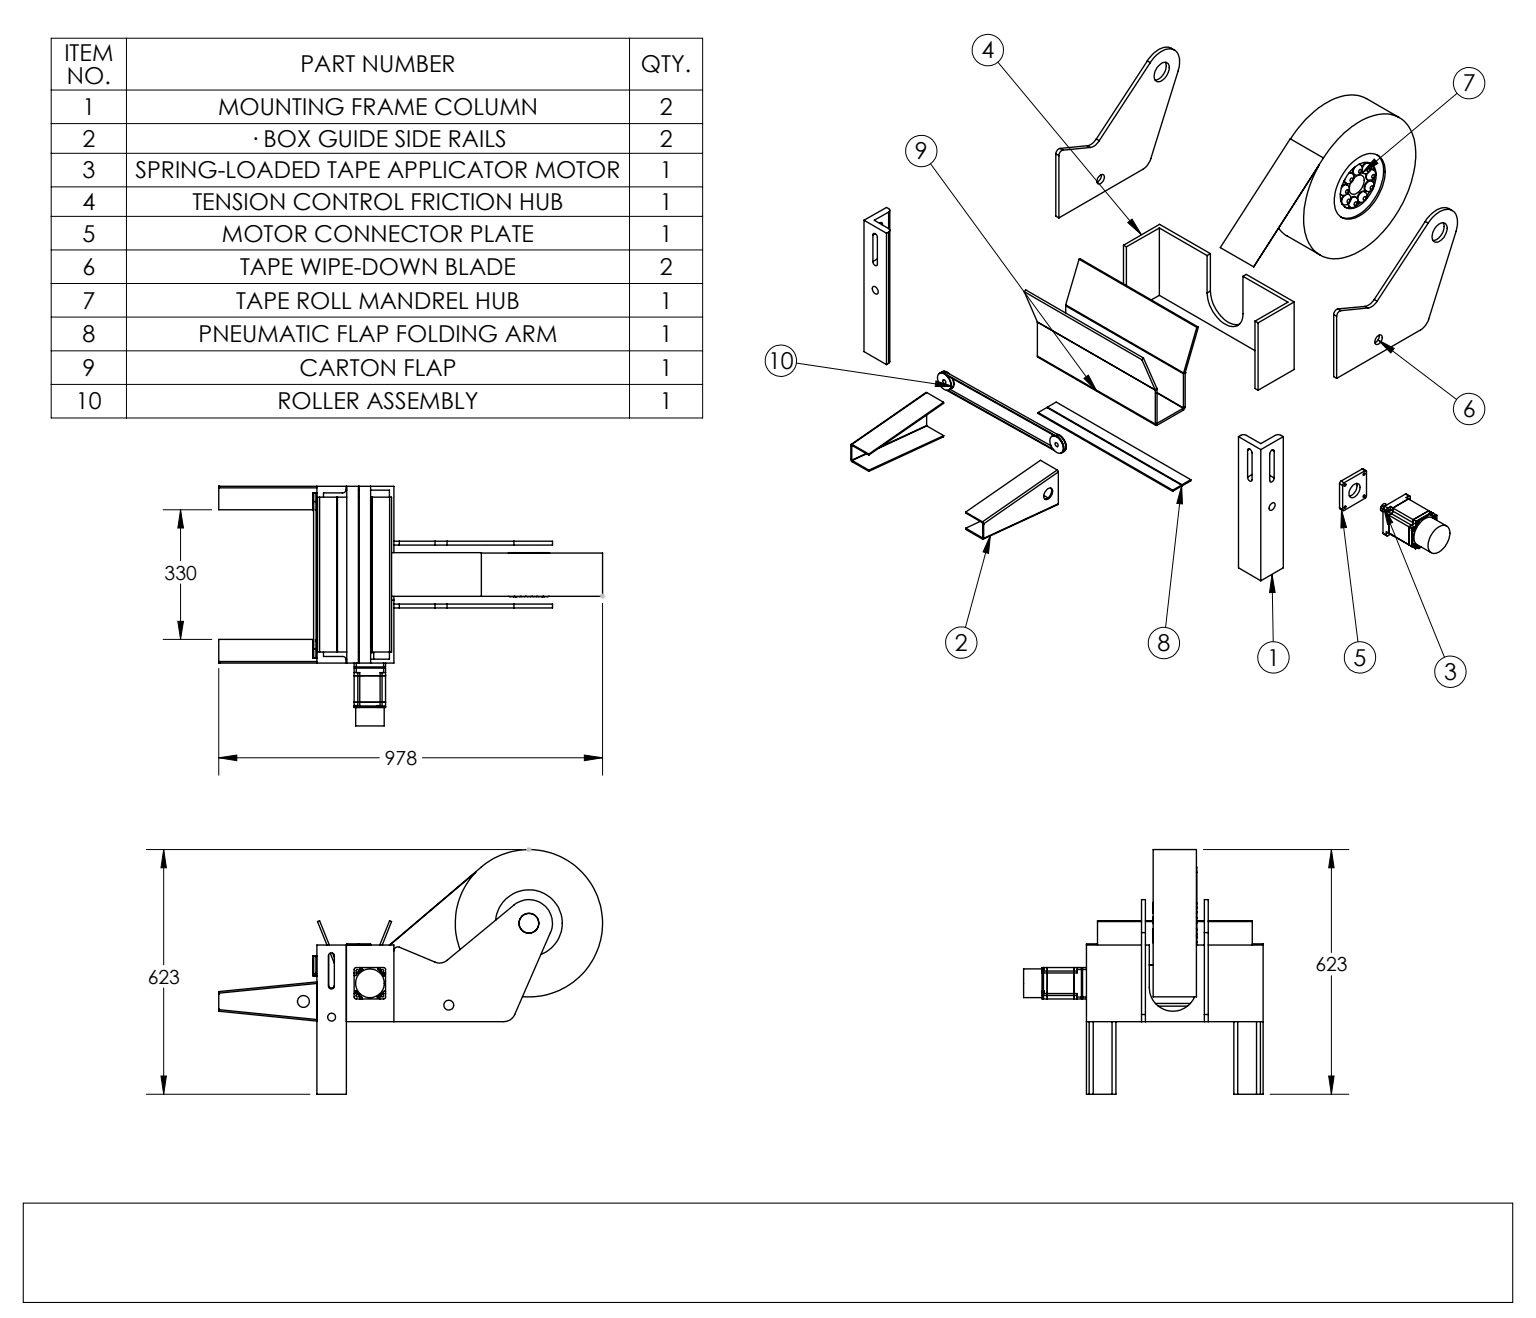
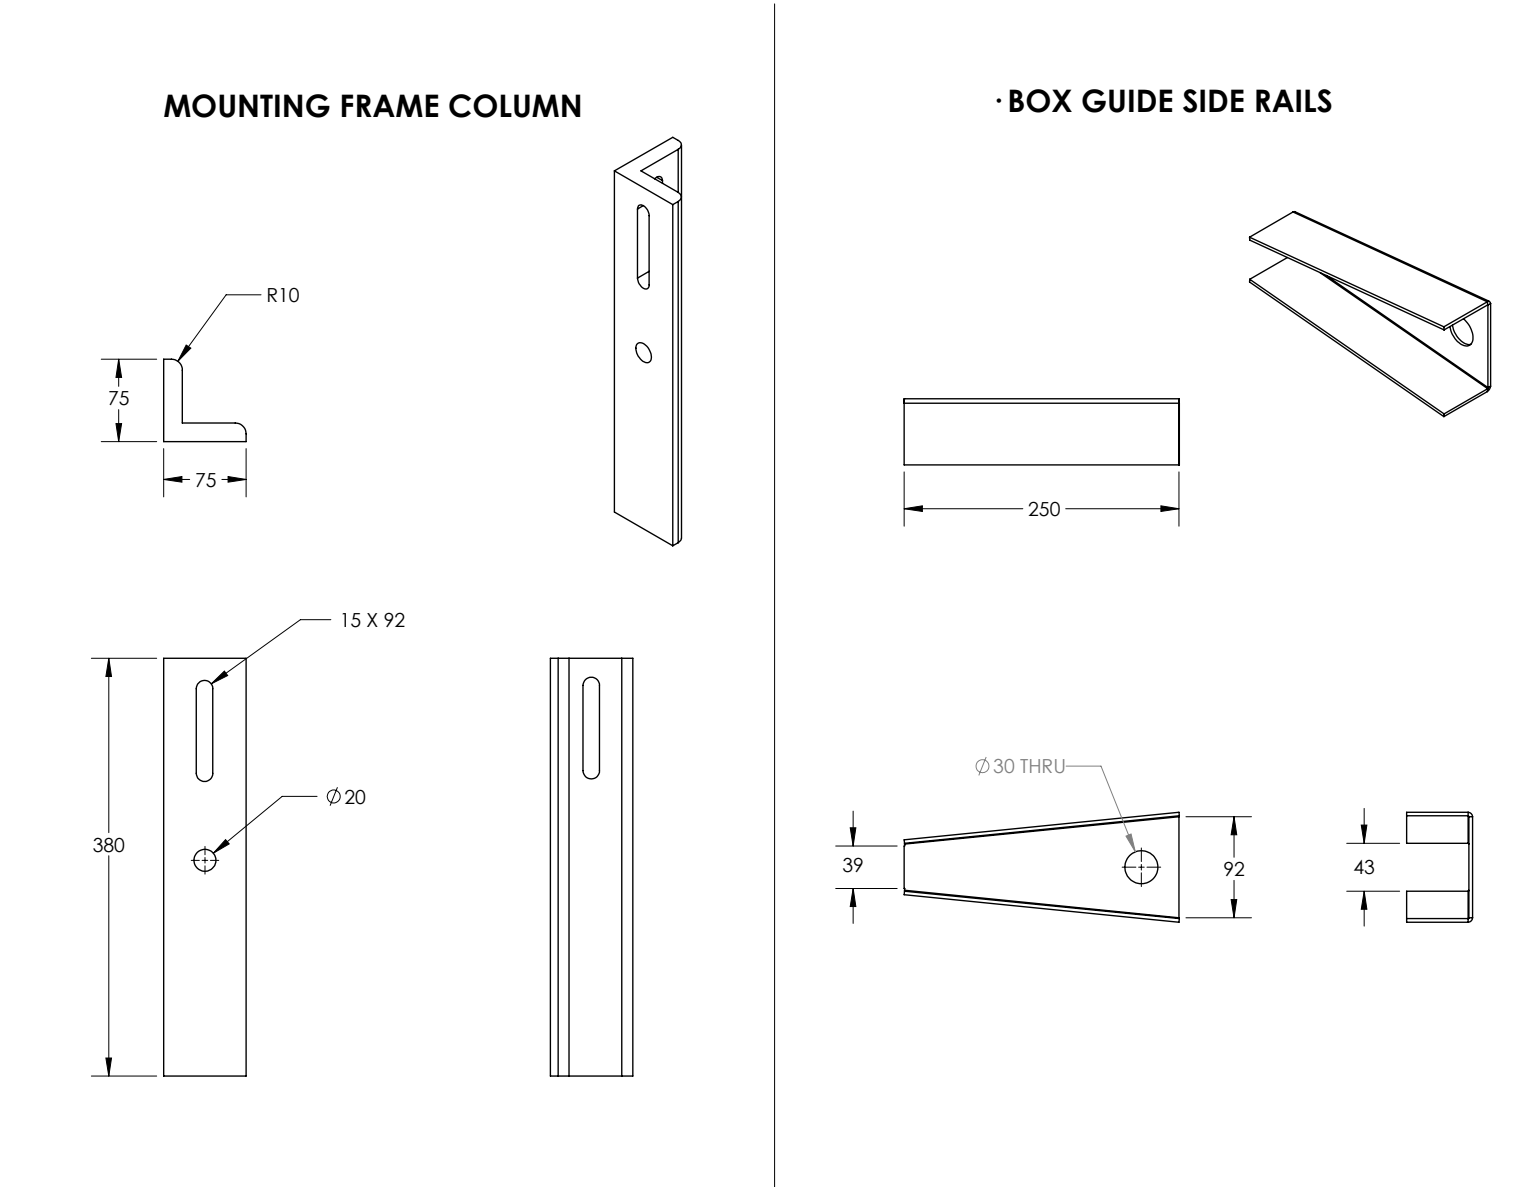
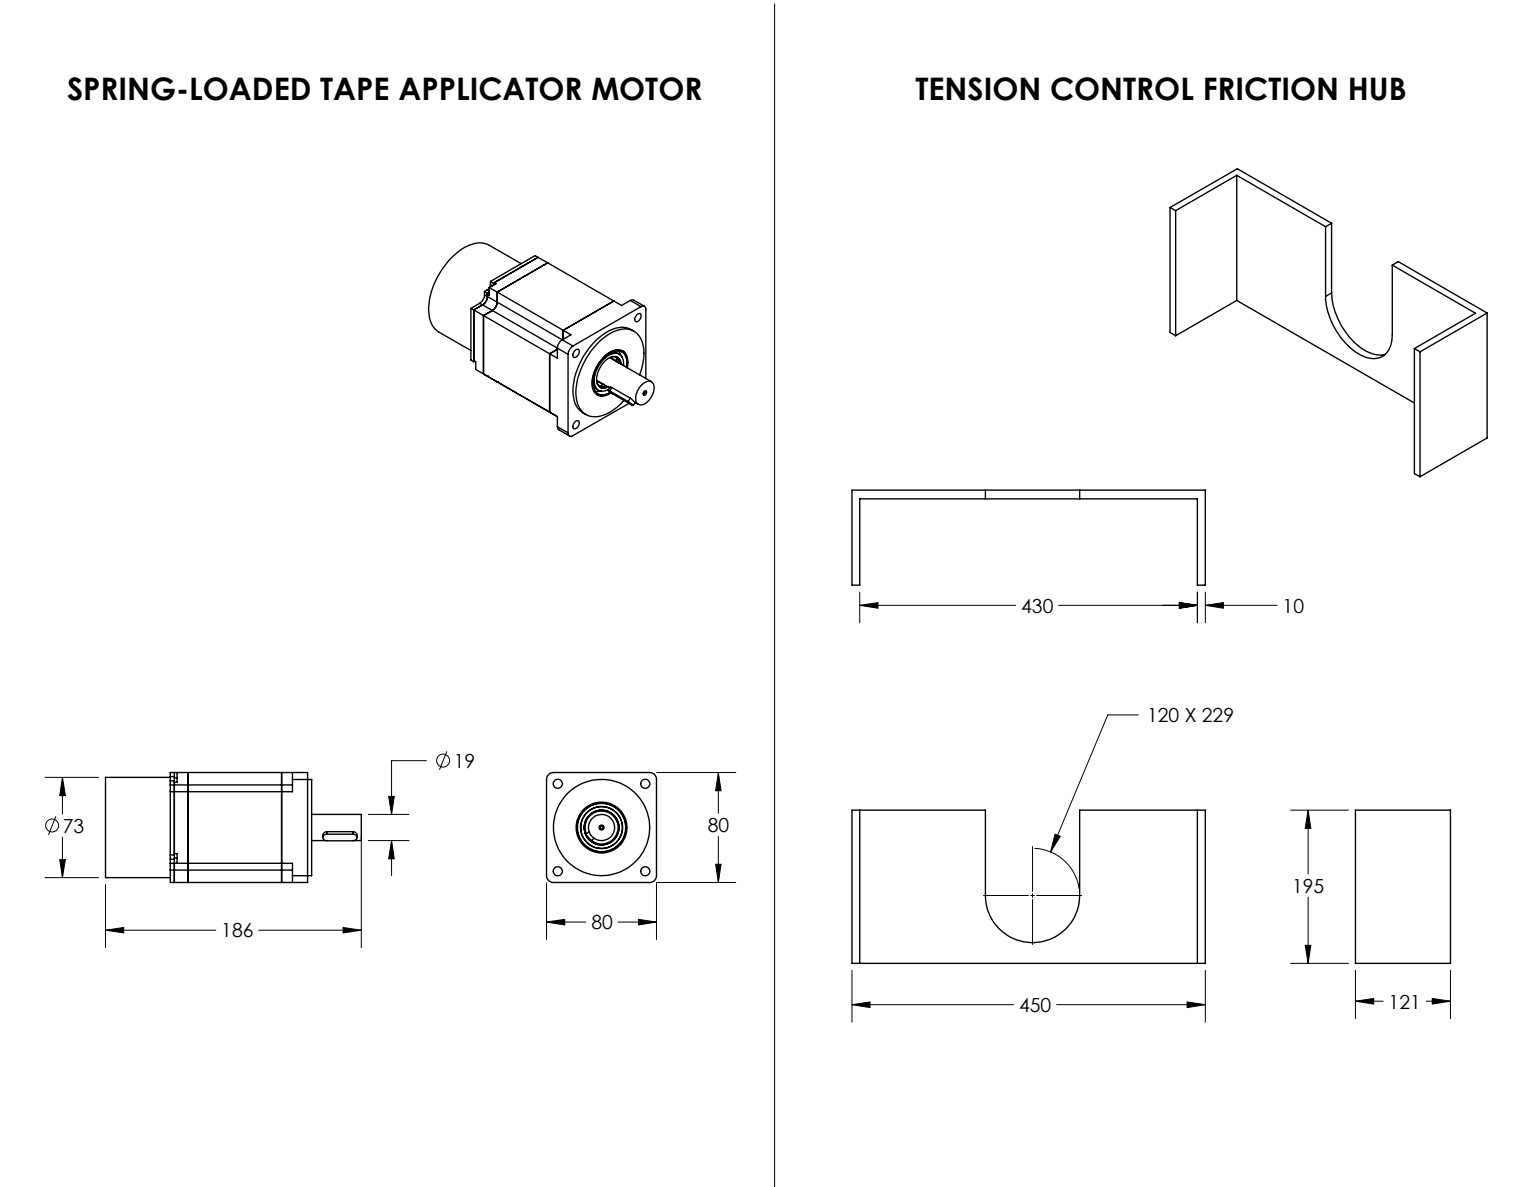
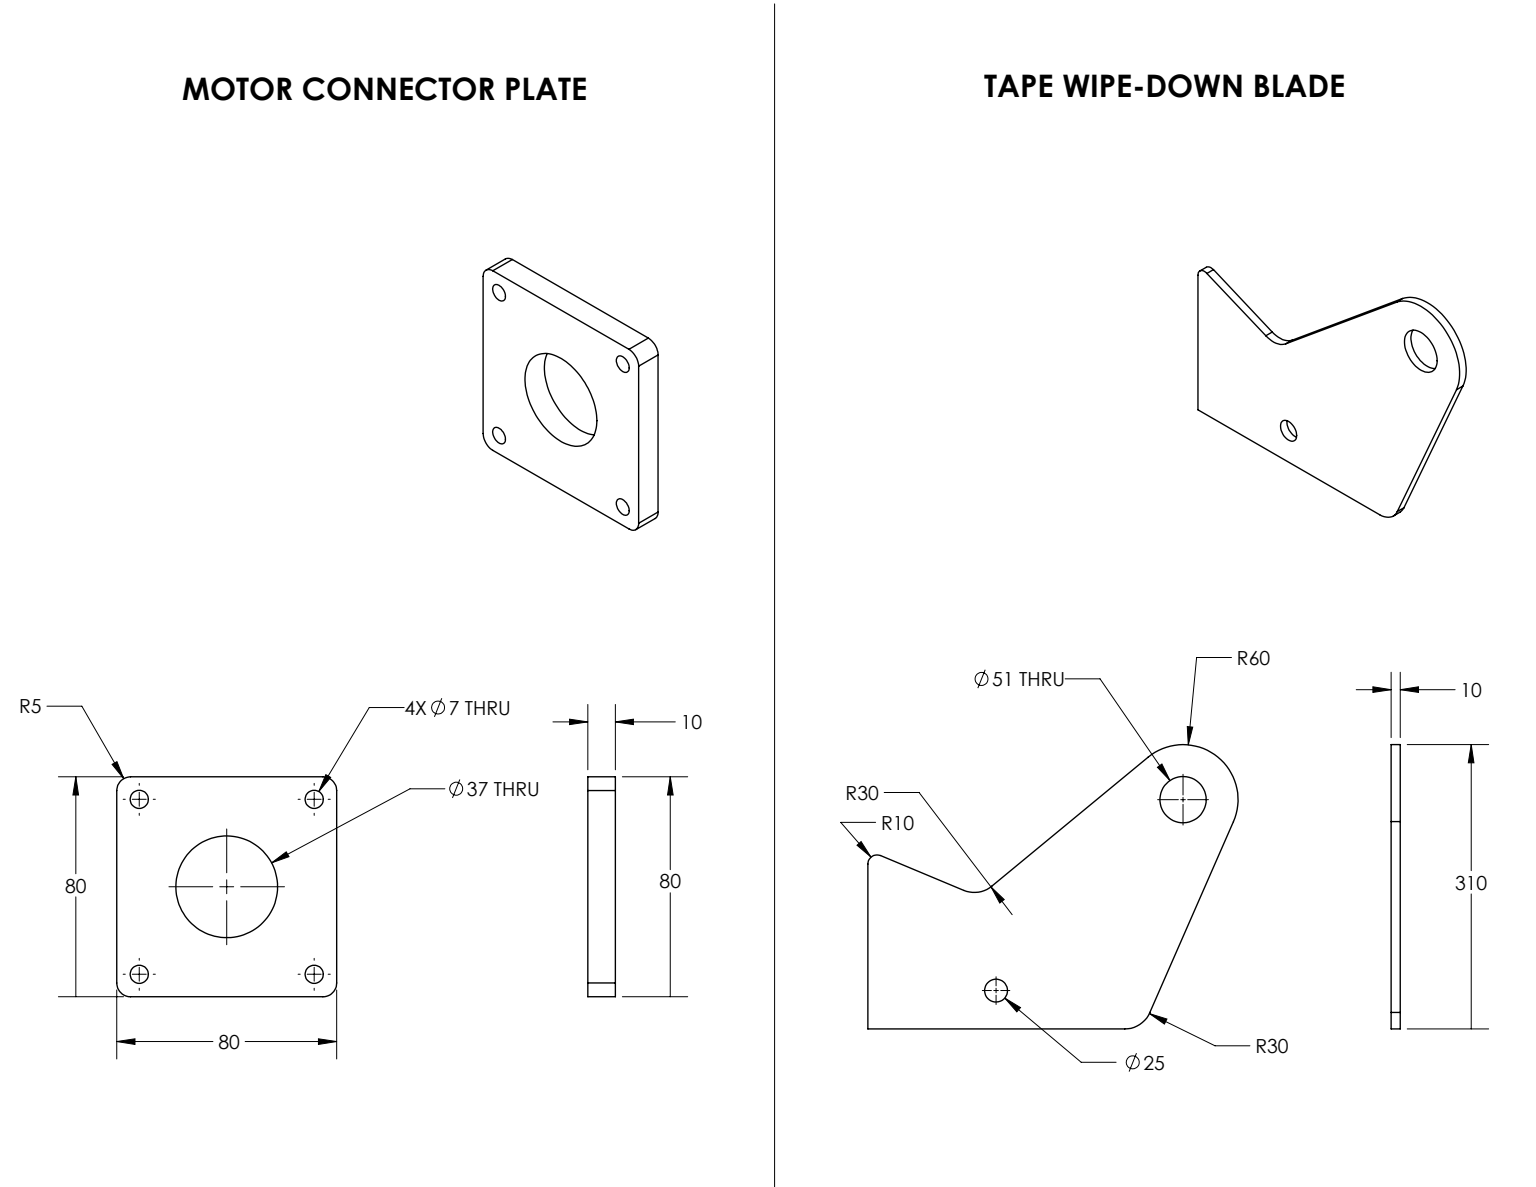
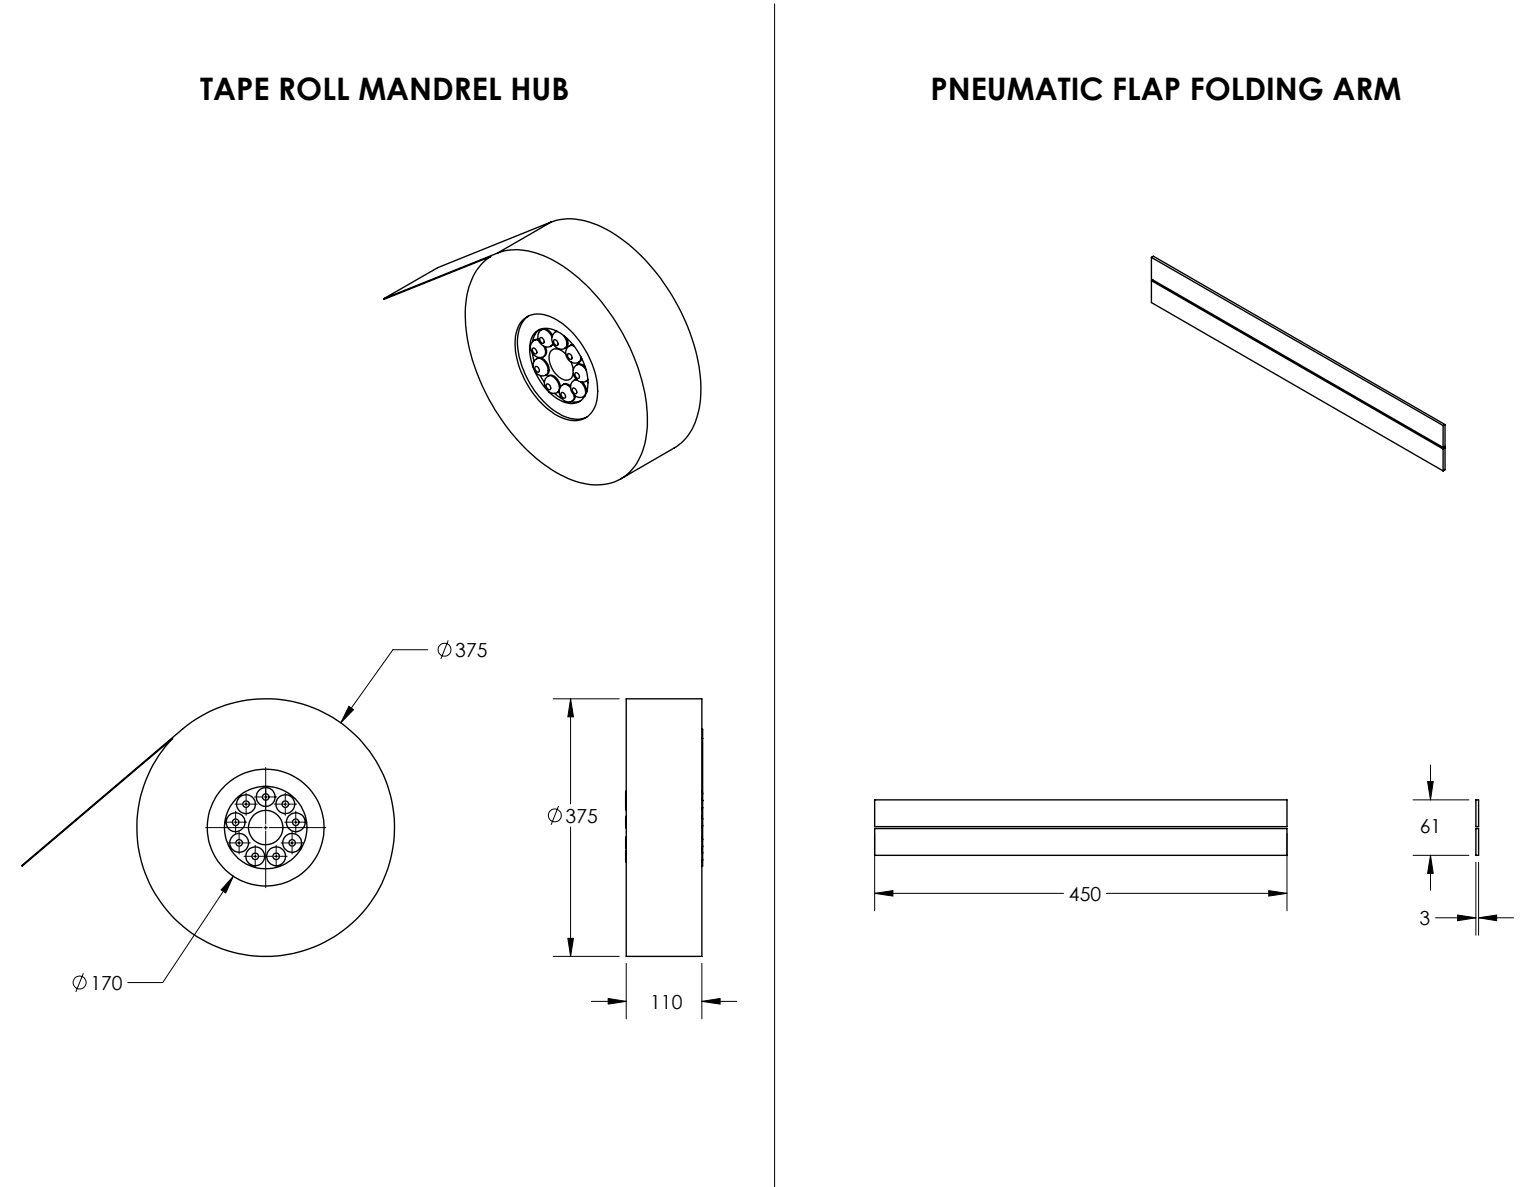
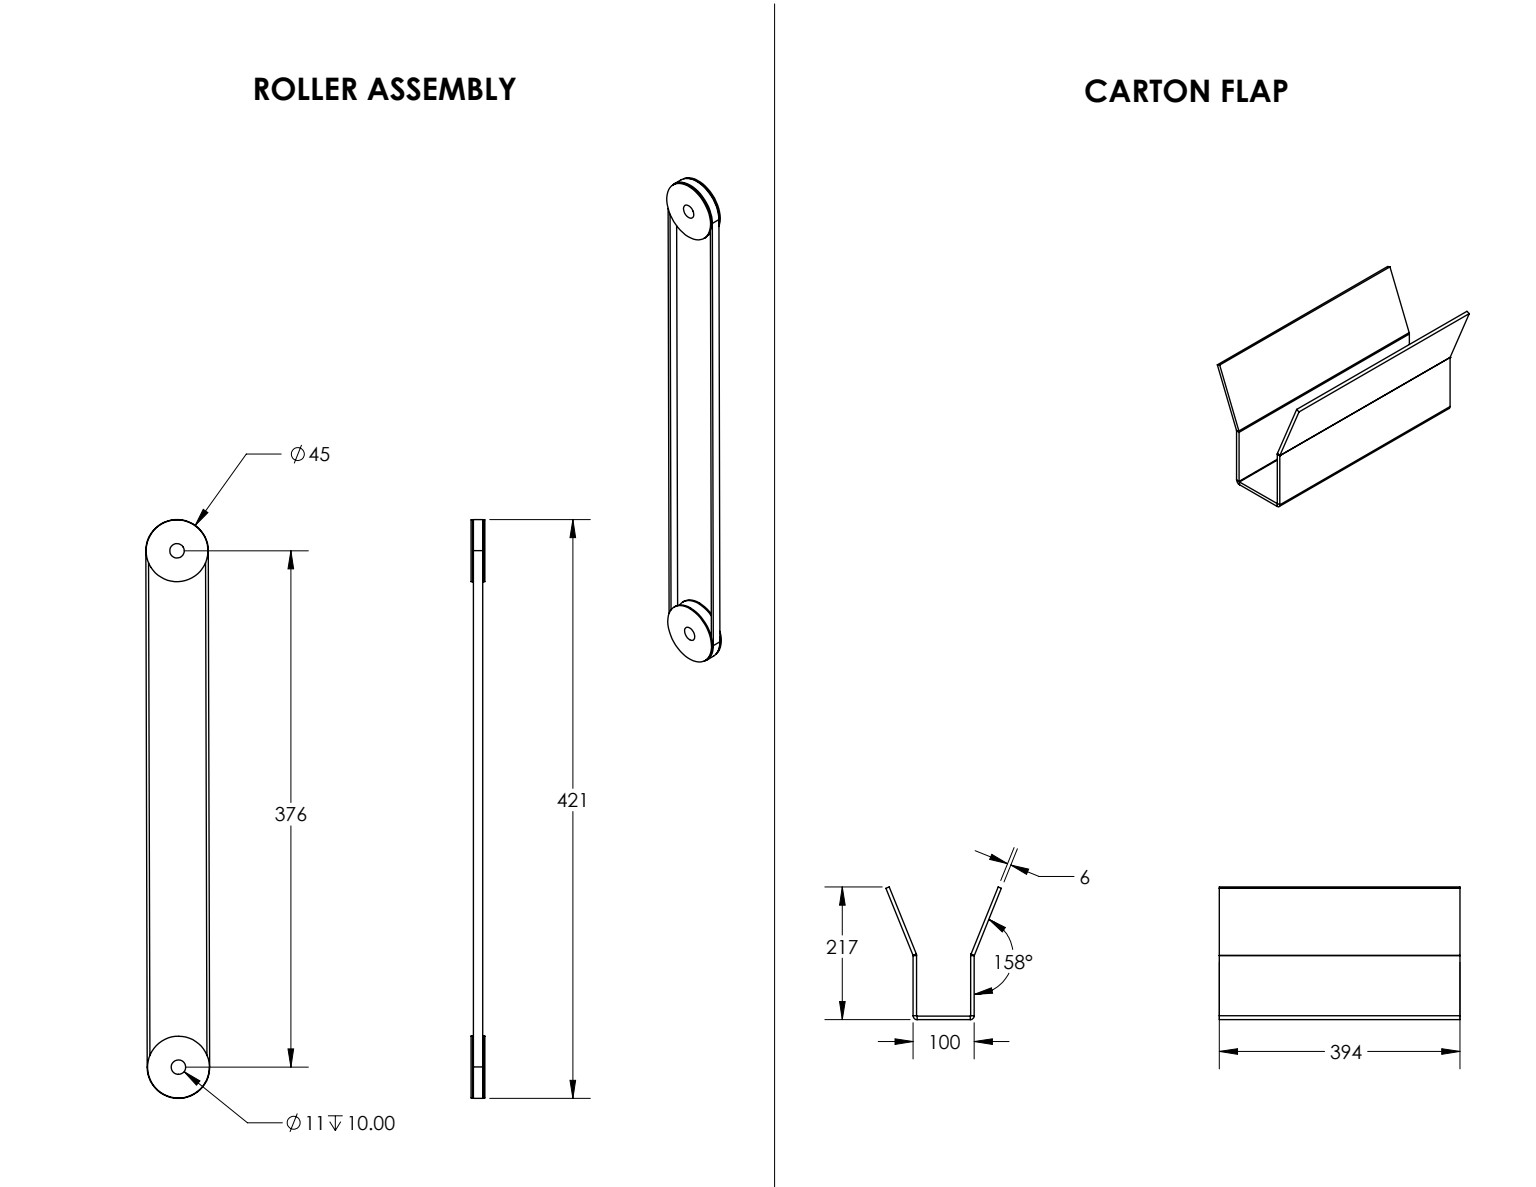
ISO-10303-21;
HEADER;
FILE_DESCRIPTION (('STEP AP214'),
    '1' );
FILE_NAME ('TAS-007',
    '2026-11-01T05:08:46',
    ( '' ),
    ( '' ),
    'SwSTEP 2.0',
    'SolidWorks 2024',
    '' );
FILE_SCHEMA (( 'AUTOMOTIVE_DESIGN' ));
ENDSEC;

DATA;
#1 = EDGE_CURVE ( 'NONE', #6268, #16000, #1193, .T. ) ;
#2 = DIRECTION ( 'NONE',  ( 1.000000000000000000, 0.000000000000000000, 0.000000000000000000 ) ) ;
#3 = ORIENTED_EDGE ( 'NONE', *, *, #13457, .T. ) ;
#4 = PLANE ( 'NONE',  #1981 ) ;
#5 = EDGE_CURVE ( 'NONE', #7189, #2938, #55, .T. ) ;
#6 = CARTESIAN_POINT ( 'NONE',  ( 55.99999999999989342, 523.2161522479888163, -507.5890438806159750 ) ) ;
#7 = ORIENTED_EDGE ( 'NONE', *, *, #1395, .F. ) ;
#8 = CARTESIAN_POINT ( 'NONE',  ( 0.000000000000000000, 10.00000000000000000, 0.000000000000000000 ) ) ;
#9 = PLANE ( 'NONE',  #8732 ) ;
#10 = CYLINDRICAL_SURFACE ( 'NONE', #6483, 2.500000000000002220 ) ;
#11 = VERTEX_POINT ( 'NONE', #11668 ) ;
#12 = CIRCLE ( 'NONE', #9067, 0.9999999999999950040 ) ;
#13 = AXIS2_PLACEMENT_3D ( 'NONE', #1699, #13214, #4196 ) ;
#14 = CARTESIAN_POINT ( 'NONE',  ( 36.99999999999999289, 6.000000000000000000, 17.99999999999998934 ) ) ;
#15 = VERTEX_POINT ( 'NONE', #6496 ) ;
#16 = EDGE_LOOP ( 'NONE', ( #11957, #12482 ) ) ;
#17 = CYLINDRICAL_SURFACE ( 'NONE', #5319, 8.000000000000000000 ) ;
#18 = PRODUCT_RELATED_PRODUCT_CATEGORY ( 'part', '', ( #10133 ) ) ;
#19 = EDGE_LOOP ( 'NONE', ( #9560, #531, #12122, #8453 ) ) ;
#20 = CARTESIAN_POINT ( 'NONE',  ( 450.0000000000000568, -58.54870895198288849, -20.17596735892307436 ) ) ;
#21 = VERTEX_POINT ( 'NONE', #5050 ) ;
#22 = EDGE_CURVE ( 'NONE', #12299, #3010, #16896, .T. ) ;
#23 = VECTOR ( 'NONE', #3492, 1000.000000000000000 ) ;
#24 = ORIENTED_EDGE ( 'NONE', *, *, #4784, .T. ) ;
#25 = SHAPE_REPRESENTATION ( 'Servo-Body.2', ( #1488 ), #13563 ) ;
#26 = CARTESIAN_POINT ( 'NONE',  ( 56.72999999999999687, 290.3130897954761735, 29.03130897954726564 ) ) ;
#27 = LINE ( 'NONE', #2765, #10533 ) ;
#28 = ORIENTED_EDGE ( 'NONE', *, *, #16422, .T. ) ;
#29 = DIRECTION ( 'NONE',  ( 0.000000000000000000, 1.000000000000000000, 0.000000000000000000 ) ) ;
#30 = DIRECTION ( 'NONE',  ( 0.000000000000000000, 1.000000000000000000, 0.000000000000000000 ) ) ;
#31 = CARTESIAN_POINT ( 'NONE',  ( 0.000000000000000000, 381.0487089519837127, -150.0000000000032685 ) ) ;
#32 = ORIENTED_EDGE ( 'NONE', *, *, #4689, .T. ) ;
#33 = DIRECTION ( 'NONE',  ( -1.000000000000000000, 0.000000000000000000, 0.000000000000000000 ) ) ;
#34 = LINE ( 'NONE', #2692, #9964 ) ;
#35 = ORIENTED_EDGE ( 'NONE', *, *, #6969, .T. ) ;
#36 = CIRCLE ( 'NONE', #12381, 84.99999999999997158 ) ;
#37 = ADVANCED_FACE ( 'NONE', ( #11495 ), #14331, .T. ) ;
#38 = FACE_OUTER_BOUND ( 'NONE', #10293, .T. ) ;
#39 = ORIENTED_EDGE ( 'NONE', *, *, #11105, .T. ) ;
#40 = DIRECTION ( 'NONE',  ( 1.000000000000000000, 0.000000000000000000, 0.000000000000000000 ) ) ;
#41 = EDGE_LOOP ( 'NONE', ( #1382, #8433, #6479, #15519 ) ) ;
#42 = EDGE_CURVE ( 'NONE', #687, #1391, #10203, .T. ) ;
#43 = ORIENTED_EDGE ( 'NONE', *, *, #5912, .T. ) ;
#44 = FILL_AREA_STYLE_COLOUR ( '', #16509 ) ;
#45 = ADVANCED_FACE ( 'NONE', ( #6580 ), #11842, .F. ) ;
#46 = DIRECTION ( 'NONE',  ( 1.000000000000000000, 0.000000000000000000, 0.000000000000000000 ) ) ;
#47 = LINE ( 'NONE', #6217, #13812 ) ;
#48 = VECTOR ( 'NONE', #5957, 1000.000000000000000 ) ;
#49 = VERTEX_POINT ( 'NONE', #336 ) ;
#50 = FACE_OUTER_BOUND ( 'NONE', #13064, .T. ) ;
#51 = PRODUCT_DEFINITION_CONTEXT ( 'detailed design', #7403, 'design' ) ;
#52 = DIRECTION ( 'NONE',  ( 3.854941057726249930E-16, 0.000000000000000000, -1.000000000000000000 ) ) ;
#53 = B_SPLINE_CURVE_WITH_KNOTS ( 'NONE', 3,
 ( #5779, #7371, #12713, #3697, #6084, #4964, #16576, #10218, #14084, #11332 ),
 .UNSPECIFIED., .F., .F.,
 ( 4, 2, 2, 2, 4 ),
 ( 0.000000000000000000, 0.2500000000000000000, 0.5000000000000000000, 0.7500000000000000000, 1.000000000000000000 ),
 .UNSPECIFIED. ) ;
#54 = DIRECTION ( 'NONE',  ( 0.000000000000000000, 0.000000000000000000, -1.000000000000000000 ) ) ;
#55 = CIRCLE ( 'NONE', #10737, 4.000000000000000000 ) ;
#56 = VECTOR ( 'NONE', #6748, 1000.000000000000000 ) ;
#57 = FACE_OUTER_BOUND ( 'NONE', #15160, .T. ) ;
#58 = CARTESIAN_POINT ( 'NONE',  ( 25.99999999999996092, 3.000000000000000000, 40.00000000000000711 ) ) ;
#59 = EDGE_CURVE ( 'NONE', #4001, #7250, #15126, .T. ) ;
#60 = PLANE ( 'NONE',  #664 ) ;
#61 = CARTESIAN_POINT ( 'NONE',  ( 35.99999999999999289, 10.00000000000000000, 17.99999999999998934 ) ) ;
#63 = EDGE_LOOP ( 'NONE', ( #16636, #11334, #7139, #11945 ) ) ;
#62 = ORIENTED_EDGE ( 'NONE', *, *, #2061, .T. ) ;
#64 = DIRECTION ( 'NONE',  ( 0.000000000000000000, 1.000000000000000000, -2.081668171172169746E-16 ) ) ;
#65 = EDGE_CURVE ( 'NONE', #15220, #14044, #10978, .T. ) ;
#66 = EDGE_CURVE ( 'NONE', #15272, #6025, #13499, .T. ) ;
#67 = EDGE_CURVE ( 'NONE', #12951, #10672, #5562, .T. ) ;
#68 = FACE_OUTER_BOUND ( 'NONE', #5126, .T. ) ;
#69 = EDGE_CURVE ( 'NONE', #1150, #1326, #513, .T. ) ;
#70 = VECTOR ( 'NONE', #318, 1000.000000000000000 ) ;
#71 = VECTOR ( 'NONE', #2, 1000.000000000000000 ) ;
#72 = CARTESIAN_POINT ( 'NONE',  ( -46.99999999999988631, 493.2350855268092573, -580.5705369404290650 ) ) ;
#73 = DIRECTION ( 'NONE',  ( 0.000000000000000000, 0.000000000000000000, -1.000000000000000000 ) ) ;
#74 = EDGE_LOOP ( 'NONE', ( #10191, #4537, #11740, #10605, #6222, #2610, #6694, #4474, #3337 ) ) ;
#75 = DIRECTION ( 'NONE',  ( -1.000000000000000000, 0.000000000000000000, 0.000000000000000000 ) ) ;
#76 = APPLICATION_CONTEXT ( 'automotive_design' ) ;
#77 = AXIS2_PLACEMENT_3D ( 'NONE', #8422, #7109, #16564 ) ;
#78 = DIRECTION ( 'NONE',  ( -1.000000000000000000, 0.000000000000000000, 0.000000000000000000 ) ) ;
#79 = ORIENTED_EDGE ( 'NONE', *, *, #8581, .F. ) ;
#80 = CARTESIAN_POINT ( 'NONE',  ( -46.99999999999988631, 523.2161522479888163, -502.8936384967199729 ) ) ;
#81 = DIRECTION ( 'NONE',  ( -1.000000000000000000, 0.000000000000000000, 0.000000000000000000 ) ) ;
#82 = ORIENTED_EDGE ( 'NONE', *, *, #2919, .T. ) ;
#83 = CARTESIAN_POINT ( 'NONE',  ( -23.00000000000002487, 10.00000000000000000, -36.99999999999999289 ) ) ;
#84 = VECTOR ( 'NONE', #15689, 1000.000000000000000 ) ;
#85 = CYLINDRICAL_SURFACE ( 'NONE', #16920, 13.69540538389601991 ) ;
#86 = CARTESIAN_POINT ( 'NONE',  ( 0.5437585709472483320, 286.2028147183448823, 37.27096646979387629 ) ) ;
#87 = ORIENTED_EDGE ( 'NONE', *, *, #7823, .T. ) ;
#88 = CARTESIAN_POINT ( 'NONE',  ( 394.0000000000001137, 339.1725919290087745, -9.945665743359786148 ) ) ;
#89 = AXIS2_PLACEMENT_3D ( 'NONE', #16436, #15148, #1397 ) ;
#90 = EDGE_CURVE ( 'NONE', #3294, #11672, #5469, .T. ) ;
#91 = FACE_OUTER_BOUND ( 'NONE', #74, .T. ) ;
#92 = CIRCLE ( 'NONE', #3112, 15.14120580695350071 ) ;
#93 = ORIENTED_EDGE ( 'NONE', *, *, #501, .T. ) ;
#94 = VECTOR ( 'NONE', #8988, 1000.000000000000000 ) ;
#95 = DIRECTION ( 'NONE',  ( 0.000000000000000000, 0.000000000000000000, -1.000000000000000000 ) ) ;
#96 = DIRECTION ( 'NONE',  ( -1.000000000000000000, -0.000000000000000000, -0.000000000000000000 ) ) ;
#97 = DIRECTION ( 'NONE',  ( 0.000000000000000000, 1.000000000000000000, 0.000000000000000000 ) ) ;
#98 = ORIENTED_EDGE ( 'NONE', *, *, #11496, .T. ) ;
#99 = CARTESIAN_POINT ( 'NONE',  ( 39.72345254347678889, 303.2115381654813859, -6.736600000000000144 ) ) ;
#100 = DIRECTION ( 'NONE',  ( 3.491481338843133355E-15, -0.9950371902099891530, -0.09950371902099770793 ) ) ;
#101 = LINE ( 'NONE', #5412, #10344 ) ;
#102 = EDGE_LOOP ( 'NONE', ( #5249, #13534 ) ) ;
#103 = AXIS2_PLACEMENT_3D ( 'NONE', #2236, #11104, #4571 ) ;
#104 = DIRECTION ( 'NONE',  ( 1.000000000000000000, 0.000000000000000000, 0.000000000000000000 ) ) ;
#105 = ORIENTED_EDGE ( 'NONE', *, *, #15495, .F. ) ;
#106 = ORIENTED_EDGE ( 'NONE', *, *, #6625, .F. ) ;
#107 = AXIS2_PLACEMENT_3D ( 'NONE', #13523, #4147, #12231 ) ;
#108 = PLANE ( 'NONE',  #4503 ) ;
#109 = AXIS2_PLACEMENT_3D ( 'NONE', #15496, #14284, #3731 ) ;
#110 = ORIENTED_EDGE ( 'NONE', *, *, #957, .T. ) ;
#111 = CIRCLE ( 'NONE', #1754, 6.473199999999998511 ) ;
#112 = ORIENTED_EDGE ( 'NONE', *, *, #11806, .F. ) ;
#113 =( NAMED_UNIT ( * ) SI_UNIT ( $, .STERADIAN. ) SOLID_ANGLE_UNIT ( ) );
#114 = AXIS2_PLACEMENT_3D ( 'NONE', #9847, #2332, #2672 ) ;
#115 = ORIENTED_EDGE ( 'NONE', *, *, #13843, .T. ) ;
#116 = AXIS2_PLACEMENT_3D ( 'NONE', #10320, #2489, #3792 ) ;
#117 = VERTEX_POINT ( 'NONE', #2818 ) ;
#118 = CARTESIAN_POINT ( 'NONE',  ( 55.99999999999989342, 493.2350855268086320, -503.4847040861888559 ) ) ;
#119 = DIRECTION ( 'NONE',  ( 0.000000000000000000, 0.000000000000000000, -1.000000000000000000 ) ) ;
#120 = CIRCLE ( 'NONE', #5038, 4.000000000000007105 ) ;
#121 = ORIENTED_EDGE ( 'NONE', *, *, #14551, .T. ) ;
#122 = DIRECTION ( 'NONE',  ( 0.000000000000000000, 0.000000000000000000, 1.000000000000000000 ) ) ;
#123 = PLANE ( 'NONE',  #5672 ) ;
#124 = ORIENTED_EDGE ( 'NONE', *, *, #2973, .T. ) ;
#125 = AXIS2_PLACEMENT_3D ( 'NONE', #6705, #364, #11958 ) ;
#126 = SURFACE_SIDE_STYLE ('',( #8186 ) ) ;
#127 = ORIENTED_EDGE ( 'NONE', *, *, #13187, .F. ) ;
#128 = FACE_BOUND ( 'NONE', #8268, .T. ) ;
#129 = DIRECTION ( 'NONE',  ( 0.000000000000000000, -1.000000000000000000, -1.321694076934710402E-16 ) ) ;
#130 = ORIENTED_EDGE ( 'NONE', *, *, #10730, .F. ) ;
#131 = DIRECTION ( 'NONE',  ( 0.000000000000000000, 0.000000000000000000, -1.000000000000000000 ) ) ;
#132 = ORIENTED_EDGE ( 'NONE', *, *, #8673, .T. ) ;
#133 = DIRECTION ( 'NONE',  ( 0.000000000000000000, 1.000000000000000000, 7.137148015447440312E-15 ) ) ;
#134 = AXIS2_PLACEMENT_3D ( 'NONE', #15085, #13801, #7423 ) ;
#135 = SHAPE_REPRESENTATION ( 'Part2', ( #1488 ), #2021 ) ;
#136 = EDGE_LOOP ( 'NONE', ( #13125, #124, #7060, #6376 ) ) ;
#137 = ORIENTED_EDGE ( 'NONE', *, *, #15607, .T. ) ;
#138 = FACE_OUTER_BOUND ( 'NONE', #14559, .T. ) ;
#139 = VECTOR ( 'NONE', #7023, 1000.000000000000000 ) ;
#140 = CARTESIAN_POINT ( 'NONE',  ( 0.000000000000000000, 372.8685141053778693, -83.18019484660869978 ) ) ;
#141 = DIRECTION ( 'NONE',  ( 0.000000000000000000, 1.000000000000000000, 0.000000000000000000 ) ) ;
#142 = ORIENTED_EDGE ( 'NONE', *, *, #15134, .F. ) ;
#143 = EDGE_CURVE ( 'NONE', #14752, #3203, #1424, .T. ) ;
#144 = CARTESIAN_POINT ( 'NONE',  ( -39.99999999999997868, 3.000000000000000000, -19.99999999999999645 ) ) ;
#145 = CARTESIAN_POINT ( 'NONE',  ( 39.99999999999999289, 10.00000000000000000, 26.00000000000000000 ) ) ;
#146 = VECTOR ( 'NONE', #14491, 1000.000000000000000 ) ;
#147 = LINE ( 'NONE', #6904, #3585 ) ;
#148 = DIRECTION ( 'NONE',  ( -0.000000000000000000, -1.000000000000000000, 0.000000000000000000 ) ) ;
#149 = DIRECTION ( 'NONE',  ( 0.000000000000000000, 0.000000000000000000, -1.000000000000000000 ) ) ;
#150 = EDGE_CURVE ( 'NONE', #6128, #3161, #9700, .T. ) ;
#151 = AXIS2_PLACEMENT_3D ( 'NONE', #9424, #3927, #10623 ) ;
#152 = CARTESIAN_POINT ( 'NONE',  ( -2.220446049250313081E-13, 135.5000000000000000, 3.000000000000000000 ) ) ;
#153 = LINE ( 'NONE', #237, #1917 ) ;
#155 = VERTEX_POINT ( 'NONE', #13316 ) ;
#154 = ORIENTED_EDGE ( 'NONE', *, *, #9509, .T. ) ;
#156 = DIRECTION ( 'NONE',  ( 0.000000000000000000, 0.000000000000000000, 1.000000000000000000 ) ) ;
#157 = CARTESIAN_POINT ( 'NONE',  ( 20.99999999999996092, 3.000000000000000000, 37.50000000000001421 ) ) ;
#158 = DIRECTION ( 'NONE',  ( 1.000000000000000000, 0.000000000000000000, 0.000000000000000000 ) ) ;
#159 = DIRECTION ( 'NONE',  ( -1.000000000000000000, -0.000000000000000000, -0.000000000000000000 ) ) ;
#160 = ORIENTED_EDGE ( 'NONE', *, *, #15589, .F. ) ;
#161 = ADVANCED_FACE ( 'NONE', ( #5735 ), #14936, .F. ) ;
#162 = CIRCLE ( 'NONE', #11396, 13.69540538389601991 ) ;
#163 = CARTESIAN_POINT ( 'NONE',  ( 394.0000000000001137, 240.0523724647196389, -110.6822657433598067 ) ) ;
#164 = CARTESIAN_POINT ( 'NONE',  ( 175.0000000000000568, 515.4878487013597805, -546.7230258972048205 ) ) ;
#165 = ORIENTED_EDGE ( 'NONE', *, *, #15092, .T. ) ;
#166 = DIRECTION ( 'NONE',  ( 1.000000000000000000, 0.000000000000000000, 0.000000000000000000 ) ) ;
#167 = EDGE_CURVE ( 'NONE', #13498, #8853, #6611, .T. ) ;
#168 = CARTESIAN_POINT ( 'NONE',  ( -26.00000000000002132, 0.000000000000000000, 40.00000000000000711 ) ) ;
#169 = CARTESIAN_POINT ( 'NONE',  ( -23.00000000000003197, 3.000000000000000000, 34.00000000000000711 ) ) ;
#170 = EDGE_CURVE ( 'NONE', #13772, #6368, #9349, .T. ) ;
#171 = ADVANCED_FACE ( 'NONE', ( #7019, #14589, #1619, #3175, #12191, #9441 ), #16134, .T. ) ;
#172 = CARTESIAN_POINT ( 'NONE',  ( -22.99999999999999645, 0.000000000000000000, 37.00000000000002132 ) ) ;
#173 = DIRECTION ( 'NONE',  ( -1.000000000000000000, -0.000000000000000000, 0.000000000000000000 ) ) ;
#174 = CARTESIAN_POINT ( 'NONE',  ( -46.99999999999988631, 473.6663340069158039, -557.2494070140132862 ) ) ;
#175 = VERTEX_POINT ( 'NONE', #3080 ) ;
#176 = AXIS2_PLACEMENT_3D ( 'NONE', #3692, #15697, #1104 ) ;
#177 = DIRECTION ( 'NONE',  ( 0.000000000000000000, 0.000000000000000000, 1.000000000000000000 ) ) ;
#178 = VECTOR ( 'NONE', #11720, 1000.000000000000000 ) ;
#179 = CARTESIAN_POINT ( 'NONE',  ( -49.99999999999999289, 515.4878487013597805, -546.7230258972048205 ) ) ;
#180 = FACE_OUTER_BOUND ( 'NONE', #4687, .T. ) ;
#181 = ORIENTED_EDGE ( 'NONE', *, *, #15280, .F. ) ;
#182 = CARTESIAN_POINT ( 'NONE',  ( 55.99999999999989342, 523.2161522479893847, -590.5524132976893270 ) ) ;
#183 = UNCERTAINTY_MEASURE_WITH_UNIT (LENGTH_MEASURE( 1.000000000000000082E-05 ), #16217, 'distance_accuracy_value', 'NONE');
#184 = CYLINDRICAL_SURFACE ( 'NONE', #9745, 5.268482129199949959 ) ;
#185 = CIRCLE ( 'NONE', #2363, 35.00000000000000711 ) ;
#186 = DIRECTION ( 'NONE',  ( 1.000000000000000000, 0.000000000000000000, 0.000000000000000000 ) ) ;
#187 = ORIENTED_EDGE ( 'NONE', *, *, #2247, .T. ) ;
#188 = CARTESIAN_POINT ( 'NONE',  ( 5.425003271131650706, 0.000000000000000000, 0.000000000000000000 ) ) ;
#189 = EDGE_CURVE ( 'NONE', #1698, #9930, #6838, .T. ) ;
#190 = DIRECTION ( 'NONE',  ( 0.000000000000000000, 0.000000000000000000, 1.000000000000000000 ) ) ;
#191 = CARTESIAN_POINT ( 'NONE',  ( 31.00000000000002842, 68.00000000000000000, 26.00000000000001066 ) ) ;
#192 = ORIENTED_EDGE ( 'NONE', *, *, #5939, .F. ) ;
#193 = EDGE_CURVE ( 'NONE', #6600, #1481, #12667, .T. ) ;
#194 = EDGE_CURVE ( 'NONE', #1410, #15340, #14768, .T. ) ;
#195 = SURFACE_SIDE_STYLE ('',( #12120 ) ) ;
#196 = ORIENTED_EDGE ( 'NONE', *, *, #11498, .T. ) ;
#197 = VERTEX_POINT ( 'NONE', #10901 ) ;
#198 = LINE ( 'NONE', #13428, #14938 ) ;
#199 = VERTEX_POINT ( 'NONE', #9610 ) ;
#200 = DIRECTION ( 'NONE',  ( 1.000000000000000000, 0.000000000000000000, 0.000000000000000000 ) ) ;
#201 = VECTOR ( 'NONE', #6539, 1000.000000000000000 ) ;
#202 = AXIS2_PLACEMENT_3D ( 'NONE', #7053, #629, #9652 ) ;
#203 = ORIENTED_EDGE ( 'NONE', *, *, #1323, .T. ) ;
#204 = VERTEX_POINT ( 'NONE', #1798 ) ;
#205 = DIRECTION ( 'NONE',  ( 0.000000000000000000, 0.000000000000000000, 1.000000000000000000 ) ) ;
#206 = DIRECTION ( 'NONE',  ( 0.000000000000000000, 0.000000000000000000, -1.000000000000000000 ) ) ;
#207 =( REPRESENTATION_RELATIONSHIP ('NONE','NONE', #9356, #7676 ) REPRESENTATION_RELATIONSHIP_WITH_TRANSFORMATION ( #7629 )SHAPE_REPRESENTATION_RELATIONSHIP( ) );
#208 = ORIENTED_EDGE ( 'NONE', *, *, #16440, .T. ) ;
#209 = CARTESIAN_POINT ( 'NONE',  ( -40.00000000000000000, 19.00000000000000000, 25.99999999999999645 ) ) ;
#210 = CARTESIAN_POINT ( 'NONE',  ( 1.050000000000000044, 16.38749999999999929, 0.000000000000000000 ) ) ;
#211 = ORIENTED_EDGE ( 'NONE', *, *, #12141, .T. ) ;
#212 =( GEOMETRIC_REPRESENTATION_CONTEXT ( 3 ) GLOBAL_UNCERTAINTY_ASSIGNED_CONTEXT ( ( #10025 ) ) GLOBAL_UNIT_ASSIGNED_CONTEXT ( ( #1452, #15788, #15621 ) ) REPRESENTATION_CONTEXT ( 'NONE', 'WORKASPACE' ) );
#213 = LINE ( 'NONE', #14888, #5281 ) ;
#214 = VERTEX_POINT ( 'NONE', #8661 ) ;
#215 = DIRECTION ( 'NONE',  ( 0.000000000000000000, 0.000000000000000000, -1.000000000000000000 ) ) ;
#216 = DIRECTION ( 'NONE',  ( -0.000000000000000000, -1.000000000000000000, -0.000000000000000000 ) ) ;
#217 = ORIENTED_EDGE ( 'NONE', *, *, #4009, .F. ) ;
#218 = DIRECTION ( 'NONE',  ( -0.000000000000000000, 1.000000000000000000, -0.000000000000000000 ) ) ;
#219 = VERTEX_POINT ( 'NONE', #3420 ) ;
#220 = CARTESIAN_POINT ( 'NONE',  ( -46.99999999999988631, 559.9933750504617365, -546.7230258972048205 ) ) ;
#221 = VERTEX_POINT ( 'NONE', #7428 ) ;
#222 = STYLED_ITEM ( 'NONE', ( #8319 ), #8493 ) ;
#223 = ORIENTED_EDGE ( 'NONE', *, *, #14861, .T. ) ;
#224 = PLANE ( 'NONE',  #3358 ) ;
#225 = EDGE_CURVE ( 'NONE', #4912, #8178, #15786, .T. ) ;
#226 = DIRECTION ( 'NONE',  ( -1.000000000000000000, -0.000000000000000000, 0.000000000000000000 ) ) ;
#227 = CARTESIAN_POINT ( 'NONE',  ( -23.00000000000002487, 10.00000000000000000, -36.99999999999999289 ) ) ;
#228 = EDGE_LOOP ( 'NONE', ( #821, #15610, #9726, #13446 ) ) ;
#229 = DIRECTION ( 'NONE',  ( 1.000000000000000000, 0.000000000000000000, -0.000000000000000000 ) ) ;
#230 = DIRECTION ( 'NONE',  ( 0.000000000000000000, 0.3420201433256759294, -0.9396926207859057634 ) ) ;
#231 = EDGE_CURVE ( 'NONE', #4632, #4912, #15094, .T. ) ;
#232 = DIRECTION ( 'NONE',  ( -1.000000000000000000, -0.000000000000000000, -0.000000000000000000 ) ) ;
#233 = DIRECTION ( 'NONE',  ( 1.000000000000000000, -0.000000000000000000, 0.000000000000000000 ) ) ;
#234 = DIRECTION ( 'NONE',  ( -0.7327934916262990317, 0.6804510993672779895, 0.000000000000000000 ) ) ;
#235 = CARTESIAN_POINT ( 'NONE',  ( 55.99999999999989342, 493.2350855268086320, -508.1801094700848580 ) ) ;
#236 = VECTOR ( 'NONE', #1676, 1000.000000000000000 ) ;
#237 = CARTESIAN_POINT ( 'NONE',  ( -22.00000000000001776, 10.00000000000000000, 33.00000000000000711 ) ) ;
#239 = EDGE_LOOP ( 'NONE', ( #5498, #1229, #14459, #13552 ) ) ;
#238 = ORIENTED_EDGE ( 'NONE', *, *, #143, .T. ) ;
#240 = DIRECTION ( 'NONE',  ( -0.000000000000000000, -1.000000000000000000, -0.000000000000000000 ) ) ;
#241 = EDGE_CURVE ( 'NONE', #13085, #1073, #5982, .T. ) ;
#242 = CARTESIAN_POINT ( 'NONE',  ( -3.302699999999637814, 285.9661841259148787, 37.54929111636468519 ) ) ;
#243 = DIRECTION ( 'NONE',  ( 0.000000000000000000, 1.000000000000000000, 0.000000000000000000 ) ) ;
#244 = CARTESIAN_POINT ( 'NONE',  ( 30.99999999999997513, 10.00000000000000000, 30.99999999999999645 ) ) ;
#245 = EDGE_CURVE ( 'NONE', #1755, #1411, #11552, .T. ) ;
#246 = EDGE_LOOP ( 'NONE', ( #7986, #8833, #5081, #14451, #2592, #16759 ) ) ;
#247 = AXIS2_PLACEMENT_3D ( 'NONE', #6243, #15452, #15365 ) ;
#248 = CARTESIAN_POINT ( 'NONE',  ( -34.99999999999998579, 0.000000000000000000, 21.00000000000000355 ) ) ;
#249 = CARTESIAN_POINT ( 'NONE',  ( 30.99999999999997868, 10.00000000000000000, -30.99999999999999645 ) ) ;
#250 = ORIENTED_EDGE ( 'NONE', *, *, #16480, .F. ) ;
#251 = DIRECTION ( 'NONE',  ( -0.000000000000000000, -1.000000000000000000, -0.000000000000000000 ) ) ;
#252 = DIRECTION ( 'NONE',  ( 1.000000000000000000, -0.000000000000000000, 0.000000000000000000 ) ) ;
#253 = DIRECTION ( 'NONE',  ( 0.000000000000000000, 0.000000000000000000, -1.000000000000000000 ) ) ;
#254 = CARTESIAN_POINT ( 'NONE',  ( 55.99999999999989342, 473.6663340069158039, -561.9448123979092315 ) ) ;
#255 = LINE ( 'NONE', #13482, #2119 ) ;
#256 = CARTESIAN_POINT ( 'NONE',  ( 22.99999999999998224, 10.00000000000000000, -31.00000000000003197 ) ) ;
#257 = ORIENTED_EDGE ( 'NONE', *, *, #5085, .T. ) ;
#258 = CARTESIAN_POINT ( 'NONE',  ( 10.00000000000000000, 372.8685141053778693, -86.48019484660871115 ) ) ;
#259 = EDGE_CURVE ( 'NONE', #12691, #4652, #11398, .T. ) ;
#260 = CONTEXT_DEPENDENT_SHAPE_REPRESENTATION ( #9858, #14531 ) ;
#261 = CARTESIAN_POINT ( 'NONE',  ( -45.00000000000000000, 515.4878487013597805, -546.7230258972048205 ) ) ;
#262 = CARTESIAN_POINT ( 'NONE',  ( -55.99999999999989342, 549.5810598491749488, -561.6352214130889706 ) ) ;
#263 = EDGE_CURVE ( 'NONE', #2860, #5863, #1951, .T. ) ;
#264 = EDGE_CURVE ( 'NONE', #8649, #6752, #7174, .T. ) ;
#265 = AXIS2_PLACEMENT_3D ( 'NONE', #2009, #9585, #7241 ) ;
#266 = ORIENTED_EDGE ( 'NONE', *, *, #13819, .T. ) ;
#267 = DIRECTION ( 'NONE',  ( -0.000000000000000000, -1.000000000000000000, -0.000000000000000000 ) ) ;
#268 = LINE ( 'NONE', #15969, #4523 ) ;
#269 = PLANE ( 'NONE',  #5082 ) ;
#270 = ORIENTED_EDGE ( 'NONE', *, *, #4582, .F. ) ;
#271 = CYLINDRICAL_SURFACE ( 'NONE', #4773, 4.999999999999990230 ) ;
#272 = DIRECTION ( 'NONE',  ( -1.000000000000000000, 0.000000000000000000, -1.156482317317870344E-15 ) ) ;
#273 = CARTESIAN_POINT ( 'NONE',  ( -45.00000000000000000, 549.5810598491746077, -531.8108303813202156 ) ) ;
#274 = ORIENTED_EDGE ( 'NONE', *, *, #7860, .T. ) ;
#275 = DIRECTION ( 'NONE',  ( -0.000000000000000000, -1.000000000000000000, -0.000000000000000000 ) ) ;
#276 = VERTEX_POINT ( 'NONE', #9787 ) ;
#277 = ORIENTED_EDGE ( 'NONE', *, *, #3429, .F. ) ;
#278 = VECTOR ( 'NONE', #3201, 1000.000000000000000 ) ;
#279 = CARTESIAN_POINT ( 'NONE',  ( -31.00000000000000000, 19.00000000000000000, 30.99999999999999289 ) ) ;
#280 = EDGE_CURVE ( 'NONE', #3951, #1946, #14054, .T. ) ;
#281 = EDGE_CURVE ( 'NONE', #13251, #11864, #11062, .T. ) ;
#282 = ORIENTED_EDGE ( 'NONE', *, *, #350, .F. ) ;
#283 = APPLICATION_PROTOCOL_DEFINITION ( 'draft international standard', 'automotive_design', 1998, #5555 ) ;
#284 = ORIENTED_EDGE ( 'NONE', *, *, #16141, .F. ) ;
#285 = ADVANCED_FACE ( 'NONE', ( #926 ), #12433, .F. ) ;
#286 = EDGE_CURVE ( 'NONE', #14252, #13943, #15423, .T. ) ;
#287 = EDGE_CURVE ( 'NONE', #1978, #13400, #16248, .T. ) ;
#288 = ORIENTED_EDGE ( 'NONE', *, *, #4993, .T. ) ;
#289 = EDGE_CURVE ( 'NONE', #6952, #11437, #8821, .T. ) ;
#290 = DIRECTION ( 'NONE',  ( 1.000000000000000000, 0.000000000000000000, 0.000000000000000000 ) ) ;
#291 = DIRECTION ( 'NONE',  ( 0.000000000000000000, 1.000000000000000000, 0.000000000000000000 ) ) ;
#292 = EDGE_LOOP ( 'NONE', ( #15746, #13221 ) ) ;
#293 = CARTESIAN_POINT ( 'NONE',  ( 46.99999999999988631, 523.2161522479893847, -604.2478186815853860 ) ) ;
#294 = DIRECTION ( 'NONE',  ( 1.000000000000000000, 0.000000000000000000, 0.000000000000000000 ) ) ;
#295 = VERTEX_POINT ( 'NONE', #5816 ) ;
#296 = LINE ( 'NONE', #13440, #11603 ) ;
#297 = ORIENTED_EDGE ( 'NONE', *, *, #9912, .F. ) ;
#298 = CARTESIAN_POINT ( 'NONE',  ( 31.00000000000003553, 19.00000000000000000, 20.99999999999999289 ) ) ;
#299 = DIRECTION ( 'NONE',  ( 0.000000000000000000, 0.000000000000000000, -1.000000000000000000 ) ) ;
#300 = ORIENTED_EDGE ( 'NONE', *, *, #13299, .F. ) ;
#301 = FACE_BOUND ( 'NONE', #15224, .T. ) ;
#302 = ORIENTED_EDGE ( 'NONE', *, *, #11387, .T. ) ;
#303 =( LENGTH_UNIT ( ) NAMED_UNIT ( * ) SI_UNIT ( .MILLI., .METRE. ) );
#304 = PLANE ( 'NONE',  #11954 ) ;
#305 = ORIENTED_EDGE ( 'NONE', *, *, #6249, .T. ) ;
#306 = APPLICATION_CONTEXT ( 'automotive_design' ) ;
#307 = ORIENTED_EDGE ( 'NONE', *, *, #286, .F. ) ;
#308 = CARTESIAN_POINT ( 'NONE',  ( 55.99999999999989342, 523.2161522479888163, -516.5890438806160319 ) ) ;
#309 = ADVANCED_FACE ( 'NONE', ( #6149 ), #10481, .F. ) ;
#310 = CARTESIAN_POINT ( 'NONE',  ( 0.000000000000000000, 363.9544815475646260, -322.6258333628447872 ) ) ;
#311 = LINE ( 'NONE', #16104, #13556 ) ;
#312 = CARTESIAN_POINT ( 'NONE',  ( 394.0000000000001137, 339.1725919290084335, -104.9456657433597968 ) ) ;
#313 = DIRECTION ( 'NONE',  ( 0.000000000000000000, 0.000000000000000000, -1.000000000000000000 ) ) ;
#314 = AXIS2_PLACEMENT_3D ( 'NONE', #72, #14498, #7952 ) ;
#315 = CARTESIAN_POINT ( 'NONE',  ( 30.99999999999999645, 68.00000000000000000, 31.00000000000001066 ) ) ;
#316 = CARTESIAN_POINT ( 'NONE',  ( 31.81980515339464333, 8.000000000000000000, -31.81980515339463622 ) ) ;
#317 = LINE ( 'NONE', #2711, #1003 ) ;
#318 = DIRECTION ( 'NONE',  ( 0.000000000000000000, -1.000000000000000000, 0.000000000000000000 ) ) ;
#319 = FACE_OUTER_BOUND ( 'NONE', #3670, .T. ) ;
#320 = DIRECTION ( 'NONE',  ( -1.000000000000000000, 0.000000000000000000, -0.000000000000000000 ) ) ;
#321 = ADVANCED_FACE ( 'NONE', ( #2203 ), #6061, .T. ) ;
#323 = ORIENTED_EDGE ( 'NONE', *, *, #3232, .T. ) ;
#322 = ORIENTED_EDGE ( 'NONE', *, *, #1688, .F. ) ;
#324 = DIRECTION ( 'NONE',  ( 0.000000000000000000, 1.000000000000000000, -0.000000000000000000 ) ) ;
#325 = CIRCLE ( 'NONE', #4154, 1.800000000000000266 ) ;
#326 = CARTESIAN_POINT ( 'NONE',  ( -2.493494276500600293, 287.9232781991976822, 37.61078711647744655 ) ) ;
#327 = FACE_OUTER_BOUND ( 'NONE', #16316, .T. ) ;
#328 = FACE_OUTER_BOUND ( 'NONE', #16951, .T. ) ;
#329 = ORIENTED_EDGE ( 'NONE', *, *, #7062, .T. ) ;
#330 = VECTOR ( 'NONE', #13966, 1000.000000000000000 ) ;
#331 = CARTESIAN_POINT ( 'NONE',  ( -40.00000000000000000, 19.00000000000000000, 25.99999999999999645 ) ) ;
#332 = DIRECTION ( 'NONE',  ( 0.000000000000000000, -1.000000000000000000, 0.000000000000000000 ) ) ;
#333 = ORIENTED_EDGE ( 'NONE', *, *, #8889, .F. ) ;
#334 = LINE ( 'NONE', #2990, #5479 ) ;
#335 = DIRECTION ( 'NONE',  ( 1.000000000000000000, 0.000000000000000000, 0.000000000000000000 ) ) ;
#336 = CARTESIAN_POINT ( 'NONE',  ( 0.000000000000000000, 234.3157724647196289, -17.15546574335979813 ) ) ;
#337 = AXIS2_PLACEMENT_3D ( 'NONE', #6271, #15489, #13602 ) ;
#338 = EDGE_LOOP ( 'NONE', ( #11132, #6961, #8646, #13596 ) ) ;
#339 = CARTESIAN_POINT ( 'NONE',  ( 45.00000000000000000, 559.9933750504617365, -533.0276205133087615 ) ) ;
#340 = ORIENTED_EDGE ( 'NONE', *, *, #12230, .T. ) ;
#341 = VECTOR ( 'NONE', #13220, 1000.000000000000114 ) ;
#342 = DIRECTION ( 'NONE',  ( 0.000000000000000000, 1.000000000000000000, 0.000000000000000000 ) ) ;
#343 = AXIS2_PLACEMENT_3D ( 'NONE', #9197, #13949, #2656 ) ;
#344 = DIRECTION ( 'NONE',  ( -1.000000000000000000, -0.000000000000000000, -1.631319816340925608E-17 ) ) ;
#345 = LINE ( 'NONE', #3090, #1996 ) ;
#346 = AXIS2_PLACEMENT_3D ( 'NONE', #5063, #9108, #2577 ) ;
#347 = ORIENTED_EDGE ( 'NONE', *, *, #12525, .F. ) ;
#348 = CARTESIAN_POINT ( 'NONE',  ( 0.000000000000000000, 239.4632308570078294, 71.73739990498292229 ) ) ;
#349 = LINE ( 'NONE', #7808, #15445 ) ;
#350 = EDGE_CURVE ( 'NONE', #7005, #8783, #2806, .T. ) ;
#351 = DIRECTION ( 'NONE',  ( 0.000000000000000000, 0.000000000000000000, 1.000000000000000000 ) ) ;
#352 = VERTEX_POINT ( 'NONE', #4541 ) ;
#353 = FACE_BOUND ( 'NONE', #6381, .T. ) ;
#354 = AXIS2_PLACEMENT_3D ( 'NONE', #9251, #2799, #13200 ) ;
#355 = AXIS2_PLACEMENT_3D ( 'NONE', #13041, #9260, #1093 ) ;
#356 = DIRECTION ( 'NONE',  ( 0.000000000000000000, -0.000000000000000000, 1.000000000000000000 ) ) ;
#357 = DIRECTION ( 'NONE',  ( 1.000000000000000000, 0.000000000000000000, -0.000000000000000000 ) ) ;
#358 = ORIENTED_EDGE ( 'NONE', *, *, #6976, .T. ) ;
#359 = PRESENTATION_STYLE_ASSIGNMENT (( #5414 ) ) ;
#360 = ORIENTED_EDGE ( 'NONE', *, *, #4262, .F. ) ;
#361 = ORIENTED_EDGE ( 'NONE', *, *, #4535, .F. ) ;
#362 = CIRCLE ( 'NONE', #9957, 3.300000000000011369 ) ;
#363 = ADVANCED_FACE ( 'NONE', ( #16549 ), #9863, .F. ) ;
#364 = DIRECTION ( 'NONE',  ( -1.000000000000000000, -0.000000000000000000, -0.000000000000000000 ) ) ;
#365 = VERTEX_POINT ( 'NONE', #2036 ) ;
#366 = AXIS2_PLACEMENT_3D ( 'NONE', #3740, #3651, #8892 ) ;
#367 = VECTOR ( 'NONE', #10969, 1000.000000000000000 ) ;
#368 = ORIENTED_EDGE ( 'NONE', *, *, #11512, .F. ) ;
#369 = ORIENTED_EDGE ( 'NONE', *, *, #6648, .T. ) ;
#370 = DIRECTION ( 'NONE',  ( 0.000000000000000000, 0.000000000000000000, 1.000000000000000000 ) ) ;
#371 = FACE_OUTER_BOUND ( 'NONE', #10755, .T. ) ;
#372 = AXIS2_PLACEMENT_3D ( 'NONE', #13169, #29, #9227 ) ;
#373 = EDGE_CURVE ( 'NONE', #3758, #6942, #6476, .T. ) ;
#374 = ORIENTED_EDGE ( 'NONE', *, *, #4662, .T. ) ;
#375 = LINE ( 'NONE', #4332, #16544 ) ;
#376 = CARTESIAN_POINT ( 'NONE',  ( 1.574999999999999956, 0.000000000000000000, 0.000000000000000000 ) ) ;
#377 = VERTEX_POINT ( 'NONE', #14230 ) ;
#378 = AXIS2_PLACEMENT_3D ( 'NONE', #11973, #5431, #9391 ) ;
#379 = CIRCLE ( 'NONE', #6377, 2.500000000000002220 ) ;
#380 = CARTESIAN_POINT ( 'NONE',  ( -36.00000000000000711, 6.000000000000000000, -18.00000000000000355 ) ) ;
#381 = VECTOR ( 'NONE', #9762, 1000.000000000000227 ) ;
#382 = ADVANCED_FACE ( 'NONE', ( #2449 ), #5115, .F. ) ;
#383 = EDGE_LOOP ( 'NONE', ( #13190, #2417, #10435, #10848 ) ) ;
#384 = LINE ( 'NONE', #9232, #10078 ) ;
#385 = DIRECTION ( 'NONE',  ( 1.000000000000000000, -0.000000000000000000, -0.000000000000000000 ) ) ;
#386 = VERTEX_POINT ( 'NONE', #6561 ) ;
#387 = EDGE_CURVE ( 'NONE', #4246, #5336, #14308, .T. ) ;
#388 = ADVANCED_FACE ( 'NONE', ( #12778 ), #10369, .T. ) ;
#389 = CARTESIAN_POINT ( 'NONE',  ( -55.99999999999989342, 549.5810598491749488, -580.0260321808809749 ) ) ;
#390 = EDGE_LOOP ( 'NONE', ( #8951, #12399, #14198, #7983 ) ) ;
#391 =( LENGTH_UNIT ( ) NAMED_UNIT ( * ) SI_UNIT ( .MILLI., .METRE. ) );
#392 = AXIS2_PLACEMENT_3D ( 'NONE', #3542, #12730, #15386 ) ;
#393 = DIRECTION ( 'NONE',  ( -0.000000000000000000, 0.09950371902100807464, -0.9950371902099882648 ) ) ;
#394 = VERTEX_POINT ( 'NONE', #12853 ) ;
#395 = ORIENTED_EDGE ( 'NONE', *, *, #13293, .F. ) ;
#396 = DIRECTION ( 'NONE',  ( -0.9998870921963913805, -0.01502673813723916403, 0.000000000000000000 ) ) ;
#397 = CARTESIAN_POINT ( 'NONE',  ( -40.00000000000000711, 10.00000000000000000, -26.00000000000000000 ) ) ;
#398 = CARTESIAN_POINT ( 'NONE',  ( 35.00000000000000711, 19.00000000000000000, -21.00000000000000355 ) ) ;
#399 = AXIS2_PLACEMENT_3D ( 'NONE', #3157, #5967, #8549 ) ;
#400 = FACE_BOUND ( 'NONE', #5435, .T. ) ;
#401 = AXIS2_PLACEMENT_3D ( 'NONE', #16893, #5208, #2559 ) ;
#402 = DIRECTION ( 'NONE',  ( -0.000000000000000000, -1.000000000000000000, -0.000000000000000000 ) ) ;
#403 = DIRECTION ( 'NONE',  ( -0.000000000000000000, -1.000000000000000000, -0.000000000000000000 ) ) ;
#404 = EDGE_CURVE ( 'NONE', #14628, #16915, #11476, .T. ) ;
#405 = CARTESIAN_POINT ( 'NONE',  ( -55.99999999999989342, 473.6663340069157471, -545.1966447803968094 ) ) ;
#406 = DIRECTION ( 'NONE',  ( 1.000000000000000000, -0.000000000000000000, -0.000000000000000000 ) ) ;
#407 = ADVANCED_FACE ( 'NONE', ( #5026 ), #16709, .T. ) ;
#408 = AXIS2_PLACEMENT_3D ( 'NONE', #12821, #7906, #16923 ) ;
#409 = EDGE_CURVE ( 'NONE', #14941, #16656, #5188, .T. ) ;
#410 = DIRECTION ( 'NONE',  ( -1.000000000000000000, -0.000000000000000000, -0.000000000000000000 ) ) ;
#411 = TOROIDAL_SURFACE ( 'NONE', #5329, 4.695405383895982609, 9.000000000000000000 ) ;
#412 = DIRECTION ( 'NONE',  ( 0.000000000000000000, 0.000000000000000000, -1.000000000000000000 ) ) ;
#414 = VERTEX_POINT ( 'NONE', #2628 ) ;
#413 = ORIENTED_EDGE ( 'NONE', *, *, #3477, .T. ) ;
#415 = CARTESIAN_POINT ( 'NONE',  ( -46.99999999999988631, 559.9933750504617365, -551.4184312811007658 ) ) ;
#416 = AXIS2_PLACEMENT_3D ( 'NONE', #12043, #453, #4135 ) ;
#417 = DIRECTION ( 'NONE',  ( 0.000000000000000000, 1.000000000000000000, 0.000000000000000000 ) ) ;
#418 = DIRECTION ( 'NONE',  ( -1.000000000000000000, -0.000000000000000000, -0.000000000000000000 ) ) ;
#419 = PLANE ( 'NONE',  #6933 ) ;
#420 = ORIENTED_EDGE ( 'NONE', *, *, #5520, .F. ) ;
#421 = CARTESIAN_POINT ( 'NONE',  ( 21.00000000000000000, 19.00000000000000000, -31.00000000000003908 ) ) ;
#422 = LINE ( 'NONE', #9526, #6191 ) ;
#423 = ORIENTED_EDGE ( 'NONE', *, *, #8704, .F. ) ;
#424 = DIRECTION ( 'NONE',  ( 0.000000000000000000, 1.000000000000000000, 0.000000000000000000 ) ) ;
#425 = AXIS2_PLACEMENT_3D ( 'NONE', #9617, #14854, #342 ) ;
#426 = AXIS2_PLACEMENT_3D ( 'NONE', #9950, #15186, #14849 ) ;
#427 = DIRECTION ( 'NONE',  ( -1.000000000000000000, 0.000000000000000000, 0.000000000000000000 ) ) ;
#428 = DIRECTION ( 'NONE',  ( -0.000000000000000000, -0.000000000000000000, 1.000000000000000000 ) ) ;
#429 = LINE ( 'NONE', #10904, #12677 ) ;
#430 = DIRECTION ( 'NONE',  ( 1.000000000000000000, 0.000000000000000000, -0.000000000000000000 ) ) ;
#431 = DIRECTION ( 'NONE',  ( -1.000000000000000000, -0.000000000000000000, -0.000000000000000000 ) ) ;
#432 = EDGE_LOOP ( 'NONE', ( #13764, #10573, #5104, #15752 ) ) ;
#433 = LINE ( 'NONE', #5661, #11650 ) ;
#434 = PRODUCT_DEFINITION_CONTEXT ( 'detailed design', #8850, 'design' ) ;
#435 = CARTESIAN_POINT ( 'NONE',  ( -2.216159785453297477E-13, 104.2500000000000142, 3.000000000000000000 ) ) ;
#436 = VECTOR ( 'NONE', #240, 1000.000000000000000 ) ;
#437 = DIRECTION ( 'NONE',  ( -1.000000000000000000, 0.000000000000000000, 0.000000000000000000 ) ) ;
#438 = ORIENTED_EDGE ( 'NONE', *, *, #9102, .F. ) ;
#439 = DIRECTION ( 'NONE',  ( 0.000000000000000000, 0.000000000000000000, 1.000000000000000000 ) ) ;
#440 = PRODUCT ( 'Assem2', 'Assem2', '', ( #2759 ) ) ;
#441 = ADVANCED_FACE ( 'NONE', ( #14401 ), #16961, .T. ) ;
#442 = DIRECTION ( 'NONE',  ( 0.000000000000000000, 1.000000000000000000, -1.224646799147353207E-16 ) ) ;
#443 = ORIENTED_EDGE ( 'NONE', *, *, #10669, .T. ) ;
#444 = LINE ( 'NONE', #13585, #11069 ) ;
#445 = DIRECTION ( 'NONE',  ( 0.000000000000000000, 0.9271838545667883125, 0.3746065934159094613 ) ) ;
#446 = FACE_OUTER_BOUND ( 'NONE', #19, .T. ) ;
#447 = ORIENTED_EDGE ( 'NONE', *, *, #14022, .T. ) ;
#448 = AXIS2_PLACEMENT_3D ( 'NONE', #9388, #14975, #8100 ) ;
#449 = AXIS2_PLACEMENT_3D ( 'NONE', #10426, #15659, #7844 ) ;
#450 =( NAMED_UNIT ( * ) PLANE_ANGLE_UNIT ( ) SI_UNIT ( $, .RADIAN. ) );
#451 = ORIENTED_EDGE ( 'NONE', *, *, #16516, .T. ) ;
#452 = VERTEX_POINT ( 'NONE', #15766 ) ;
#453 = DIRECTION ( 'NONE',  ( -1.000000000000000000, 0.000000000000000000, -0.000000000000000000 ) ) ;
#454 = EDGE_LOOP ( 'NONE', ( #6809, #515, #4102, #6359 ) ) ;
#455 = APPLICATION_PROTOCOL_DEFINITION ( 'draft international standard', 'automotive_design', 1998, #3586 ) ;
#456 = ADVANCED_FACE ( 'NONE', ( #3832 ), #10195, .T. ) ;
#457 = ORIENTED_EDGE ( 'NONE', *, *, #6897, .F. ) ;
#458 = AXIS2_PLACEMENT_3D ( 'NONE', #2840, #8249, #10918 ) ;
#459 = ORIENTED_EDGE ( 'NONE', *, *, #16113, .T. ) ;
#460 = VECTOR ( 'NONE', #7441, 1000.000000000000000 ) ;
#461 = CARTESIAN_POINT ( 'NONE',  ( 64.99999999999998579, 0.000000000000000000, -17.00000000000000355 ) ) ;
#462 = CYLINDRICAL_SURFACE ( 'NONE', #9166, 4.006599999998678108 ) ;
#463 = EDGE_CURVE ( 'NONE', #12295, #11373, #4943, .T. ) ;
#464 = ORIENTED_EDGE ( 'NONE', *, *, #15230, .F. ) ;
#465 = DIRECTION ( 'NONE',  ( -0.000000000000000000, -1.000000000000000000, -0.000000000000000000 ) ) ;
#466 = CARTESIAN_POINT ( 'NONE',  ( 0.7365999999999761627, 286.2094592450220034, 37.20452120302223875 ) ) ;
#467 = ORIENTED_EDGE ( 'NONE', *, *, #1204, .F. ) ;
#468 = ORIENTED_EDGE ( 'NONE', *, *, #16048, .T. ) ;
#469 = DIRECTION ( 'NONE',  ( -0.000000000000000000, -1.000000000000000000, -0.000000000000000000 ) ) ;
#470 = CYLINDRICAL_SURFACE ( 'NONE', #5849, 84.99999999999997158 ) ;
#471 = ORIENTED_EDGE ( 'NONE', *, *, #2752, .T. ) ;
#472 = CIRCLE ( 'NONE', #7564, 4.695405383896011919 ) ;
#473 = VECTOR ( 'NONE', #673, 1000.000000000000000 ) ;
#474 = ORIENTED_EDGE ( 'NONE', *, *, #3207, .F. ) ;
#475 = DIRECTION ( 'NONE',  ( 1.000000000000000000, 0.000000000000000000, 0.000000000000000000 ) ) ;
#476 = EDGE_CURVE ( 'NONE', #15129, #9524, #13514, .T. ) ;
#477 = EDGE_CURVE ( 'NONE', #14542, #2235, #14154, .T. ) ;
#478 = VERTEX_POINT ( 'NONE', #11649 ) ;
#479 = ORIENTED_EDGE ( 'NONE', *, *, #12252, .F. ) ;
#480 = CARTESIAN_POINT ( 'NONE',  ( -3.000000000000000000, 41.00000000000000711, 9.013878188659973034 ) ) ;
#481 = DIRECTION ( 'NONE',  ( 0.000000000000000000, 0.000000000000000000, 1.000000000000000000 ) ) ;
#482 = ADVANCED_FACE ( 'NONE', ( #2373 ), #7600, .F. ) ;
#483 = DIRECTION ( 'NONE',  ( 0.000000000000000000, -0.000000000000000000, -1.000000000000000000 ) ) ;
#484 = VECTOR ( 'NONE', #7409, 1000.000000000000000 ) ;
#485 = EDGE_CURVE ( 'NONE', #7998, #10795, #7719, .T. ) ;
#487 = ADVANCED_FACE ( 'NONE', ( #11733 ), #3920, .F. ) ;
#486 = CARTESIAN_POINT ( 'NONE',  ( 54.99999999999999289, 515.4878487013597805, -546.7230258972048205 ) ) ;
#488 = LINE ( 'NONE', #145, #11605 ) ;
#489 = CARTESIAN_POINT ( 'NONE',  ( -3.165718926336560823, 192.4396550164971984, 37.56780454546862558 ) ) ;
#490 = LINE ( 'NONE', #9679, #7358 ) ;
#491 = LINE ( 'NONE', #13786, #10610 ) ;
#492 = CARTESIAN_POINT ( 'NONE',  ( 31.00000000000003908, 19.00000000000000000, -26.00000000000000355 ) ) ;
#493 = CARTESIAN_POINT ( 'NONE',  ( 55.99999999999989342, 549.5810598491746077, -518.1154249974242703 ) ) ;
#494 = DIRECTION ( 'NONE',  ( 0.000000000000000000, 0.000000000000000000, -1.000000000000000000 ) ) ;
#496 = ORIENTED_EDGE ( 'NONE', *, *, #6783, .T. ) ;
#495 = ORIENTED_EDGE ( 'NONE', *, *, #7517, .F. ) ;
#497 = CARTESIAN_POINT ( 'NONE',  ( 1.845421771225094210, 38.60300962669240477, 9.323305159997634206 ) ) ;
#498 = EDGE_CURVE ( 'NONE', #5425, #7059, #16112, .T. ) ;
#499 = CARTESIAN_POINT ( 'NONE',  ( -26.00000000000000000, 19.00000000000000000, 40.00000000000001421 ) ) ;
#500 = CYLINDRICAL_SURFACE ( 'NONE', #1121, 7.999999999999996447 ) ;
#501 = EDGE_CURVE ( 'NONE', #12090, #11379, #6820, .T. ) ;
#502 = CARTESIAN_POINT ( 'NONE',  ( -55.99999999999989342, 473.6663340069158039, -561.9448123979092315 ) ) ;
#503 = ADVANCED_FACE ( 'NONE', ( #14570 ), #12397, .T. ) ;
#505 = ORIENTED_EDGE ( 'NONE', *, *, #11806, .T. ) ;
#504 = EDGE_CURVE ( 'NONE', #11776, #6598, #7167, .T. ) ;
#506 = EDGE_CURVE ( 'NONE', #7981, #15905, #4356, .T. ) ;
#507 = CIRCLE ( 'NONE', #10098, 9.000000000000007105 ) ;
#508 = CARTESIAN_POINT ( 'NONE',  ( -26.00000000000002132, 10.00000000000000000, -39.99999999999999289 ) ) ;
#509 = EDGE_LOOP ( 'NONE', ( #15845, #8645 ) ) ;
#510 = DIRECTION ( 'NONE',  ( -1.000000000000000000, 0.000000000000000000, -0.000000000000000000 ) ) ;
#511 = CIRCLE ( 'NONE', #4877, 5.000000000000000888 ) ;
#512 = DIRECTION ( 'NONE',  ( -0.000000000000000000, -1.000000000000000000, -0.000000000000000000 ) ) ;
#513 = LINE ( 'NONE', #16050, #5810 ) ;
#514 = CARTESIAN_POINT ( 'NONE',  ( 32.99999999999998579, 8.000000000000000000, 25.99999999999999645 ) ) ;
#515 = ORIENTED_EDGE ( 'NONE', *, *, #5284, .F. ) ;
#516 = DIRECTION ( 'NONE',  ( 1.000000000000000000, 0.000000000000000000, 0.000000000000000000 ) ) ;
#517 = CARTESIAN_POINT ( 'NONE',  ( -1.776356839400249676E-15, 0.000000000000000000, 0.000000000000000000 ) ) ;
#518 = VECTOR ( 'NONE', #5837, 1000.000000000000000 ) ;
#519 = CARTESIAN_POINT ( 'NONE',  ( -40.00000000000000000, 19.00000000000000000, -26.00000000000000355 ) ) ;
#520 = ORIENTED_EDGE ( 'NONE', *, *, #15915, .F. ) ;
#521 = EDGE_CURVE ( 'NONE', #10509, #13944, #4186, .T. ) ;
#522 = FACE_BOUND ( 'NONE', #6433, .T. ) ;
#523 = UNCERTAINTY_MEASURE_WITH_UNIT (LENGTH_MEASURE( 1.000000000000000082E-05 ), #13317, 'distance_accuracy_value', 'NONE');
#524 = CARTESIAN_POINT ( 'NONE',  ( 55.99999999999989342, 549.5810598491749488, -575.3306267969850296 ) ) ;
#525 = ORIENTED_EDGE ( 'NONE', *, *, #3393, .T. ) ;
#526 = CARTESIAN_POINT ( 'NONE',  ( 26.00000000000000000, 11.00000000000000000, 31.00000000000003197 ) ) ;
#527 = DIRECTION ( 'NONE',  ( 1.000000000000000000, 0.000000000000000000, 0.000000000000000000 ) ) ;
#528 = LINE ( 'NONE', #10654, #16885 ) ;
#529 = VERTEX_POINT ( 'NONE', #13290 ) ;
#530 = LINE ( 'NONE', #2063, #1767 ) ;
#531 = ORIENTED_EDGE ( 'NONE', *, *, #13661, .F. ) ;
#532 = ORIENTED_EDGE ( 'NONE', *, *, #12548, .F. ) ;
#533 = CARTESIAN_POINT ( 'NONE',  ( 49.99999999999999289, 515.4878487013597805, -461.7230258972048205 ) ) ;
#534 = ORIENTED_EDGE ( 'NONE', *, *, #4637, .T. ) ;
#535 = EDGE_CURVE ( 'NONE', #6745, #7963, #6646, .T. ) ;
#536 = SHAPE_DEFINITION_REPRESENTATION ( #12591, #584 ) ;
#537 = CIRCLE ( 'NONE', #16696, 4.695405383896011919 ) ;
#538 = EDGE_LOOP ( 'NONE', ( #7042, #495 ) ) ;
#539 = CARTESIAN_POINT ( 'NONE',  ( 0.7824566857511728868, 62.90282673968097527, 9.469691317190790159 ) ) ;
#540 = EDGE_CURVE ( 'NONE', #4246, #12484, #6999, .T. ) ;
#541 = ORIENTED_EDGE ( 'NONE', *, *, #2434, .F. ) ;
#542 = CARTESIAN_POINT ( 'NONE',  ( 20.99999999999996092, 3.000000000000000000, 32.50000000000000711 ) ) ;
#543 = DIRECTION ( 'NONE',  ( 0.000000000000000000, 0.3746065934159052424, -0.9271838545667901998 ) ) ;
#544 = VERTEX_POINT ( 'NONE', #15850 ) ;
#545 = PLANE ( 'NONE',  #2000 ) ;
#546 = CARTESIAN_POINT ( 'NONE',  ( 46.99999999999988631, 549.5810598491749488, -580.0260321808809749 ) ) ;
#547 = EDGE_LOOP ( 'NONE', ( #8890, #8502, #7559, #15041 ) ) ;
#548 = VECTOR ( 'NONE', #4872, 1000.000000000000000 ) ;
#549 =( NAMED_UNIT ( * ) PLANE_ANGLE_UNIT ( ) SI_UNIT ( $, .RADIAN. ) );
#550 = ORIENTED_EDGE ( 'NONE', *, *, #4758, .F. ) ;
#551 = FACE_OUTER_BOUND ( 'NONE', #9723, .T. ) ;
#552 = ORIENTED_EDGE ( 'NONE', *, *, #4766, .T. ) ;
#553 = EDGE_CURVE ( 'NONE', #8853, #13498, #14617, .T. ) ;
#554 = ORIENTED_EDGE ( 'NONE', *, *, #9518, .T. ) ;
#555 = DIRECTION ( 'NONE',  ( -0.7976179040349732352, -1.286774331876086569E-18, -0.6031630618355671158 ) ) ;
#556 = ADVANCED_BREP_SHAPE_REPRESENTATION ( '', ( #3094, #1488 ), #5315 ) ;
#557 = ORIENTED_EDGE ( 'NONE', *, *, #10454, .T. ) ;
#558 = CIRCLE ( 'NONE', #16457, 4.000164074322309027 ) ;
#559 = ORIENTED_EDGE ( 'NONE', *, *, #8857, .F. ) ;
#560 = CARTESIAN_POINT ( 'NONE',  ( -2.901926423773061536, 40.21397019809104023, 9.046021540735431188 ) ) ;
#561 = VECTOR ( 'NONE', #5113, 1000.000000000000000 ) ;
#562 = CARTESIAN_POINT ( 'NONE',  ( 25.99999999999996092, 3.000000000000000000, -33.99999999999998579 ) ) ;
#563 = CARTESIAN_POINT ( 'NONE',  ( 45.00000000000000000, 473.6663340069157471, -531.5012393965008641 ) ) ;
#564 = VECTOR ( 'NONE', #16813, 1000.000000000000000 ) ;
#565 = CARTESIAN_POINT ( 'NONE',  ( 54.99999999999999289, 334.9272574771864015, -321.9943432880672276 ) ) ;
#566 = EDGE_CURVE ( 'NONE', #4897, #14008, #2886, .T. ) ;
#567 = PLANE ( 'NONE',  #12865 ) ;
#568 = CARTESIAN_POINT ( 'NONE',  ( -45.00000000000000000, 493.2350855268086320, -508.1801094700848580 ) ) ;
#569 = DIRECTION ( 'NONE',  ( 1.000000000000000000, 0.000000000000000000, 0.000000000000000000 ) ) ;
#570 = DIRECTION ( 'NONE',  ( -0.000000000000000000, -1.000000000000000000, -0.000000000000000000 ) ) ;
#571 = AXIS2_PLACEMENT_3D ( 'NONE', #3996, #14472, #2694 ) ;
#572 = VECTOR ( 'NONE', #9766, 1000.000000000000000 ) ;
#573 = CARTESIAN_POINT ( 'NONE',  ( 3.000000000000000000, 1.836909530733565148E-16, 22.00000000000000000 ) ) ;
#574 = DIRECTION ( 'NONE',  ( -1.000000000000000000, 3.474153781073081543E-15, -3.474153781073103631E-16 ) ) ;
#576 = ORIENTED_EDGE ( 'NONE', *, *, #14354, .T. ) ;
#575 = ORIENTED_EDGE ( 'NONE', *, *, #10890, .F. ) ;
#577 = ADVANCED_FACE ( 'NONE', ( #8127 ), #5716, .F. ) ;
#578 = LINE ( 'NONE', #3243, #14140 ) ;
#579 = CARTESIAN_POINT ( 'NONE',  ( 39.99999999999999289, 8.000000000000000000, 18.99999999999999645 ) ) ;
#580 = LINE ( 'NONE', #5728, #7140 ) ;
#581 = DIRECTION ( 'NONE',  ( -1.000000000000000000, -0.000000000000000000, -0.000000000000000000 ) ) ;
#582 = VECTOR ( 'NONE', #5460, 1000.000000000000000 ) ;
#583 = VERTEX_POINT ( 'NONE', #11907 ) ;
#584 = SHAPE_REPRESENTATION ( 'Part5', ( #1488 ), #4776 ) ;
#585 = FACE_OUTER_BOUND ( 'NONE', #12046, .T. ) ;
#587 = EDGE_CURVE ( 'NONE', #1572, #3874, #1682, .T. ) ;
#586 = EDGE_LOOP ( 'NONE', ( #4983, #9221, #13584, #12457 ) ) ;
#588 = DIRECTION ( 'NONE',  ( 0.000000000000000000, 0.000000000000000000, -1.000000000000000000 ) ) ;
#589 = EDGE_CURVE ( 'NONE', #6207, #14628, #14828, .T. ) ;
#590 = CARTESIAN_POINT ( 'NONE',  ( -39.99999999999999289, 0.000000000000000000, 34.99999999999997868 ) ) ;
#591 = DIRECTION ( 'NONE',  ( -0.000000000000000000, -1.000000000000000000, -0.000000000000000000 ) ) ;
#592 = CARTESIAN_POINT ( 'NONE',  ( 415.0210210471910841, 329.6061121441327941, 0.000000000000000000 ) ) ;
#593 = CARTESIAN_POINT ( 'NONE',  ( 21.99999999999998224, 8.000000000000000000, -32.99999999999999289 ) ) ;
#594 = VERTEX_POINT ( 'NONE', #5452 ) ;
#595 = ADVANCED_FACE ( 'NONE', ( #8292 ), #10698, .F. ) ;
#596 = EDGE_CURVE ( 'NONE', #7827, #13441, #12258, .T. ) ;
#597 = VECTOR ( 'NONE', #10608, 1000.000000000000000 ) ;
#598 = EDGE_CURVE ( 'NONE', #16829, #7102, #9508, .T. ) ;
#599 = LINE ( 'NONE', #3258, #12217 ) ;
#600 = EDGE_CURVE ( 'NONE', #13441, #16829, #10788, .T. ) ;
#601 = DIRECTION ( 'NONE',  ( 1.000000000000000000, -0.000000000000000000, -0.000000000000000000 ) ) ;
#602 = LINE ( 'NONE', #519, #12957 ) ;
#603 = EDGE_LOOP ( 'NONE', ( #196, #16739, #1318, #8530 ) ) ;
#604 = CARTESIAN_POINT ( 'NONE',  ( 2.999999999999996003, 66.00000000000000000, 9.013878188659974811 ) ) ;
#605 = VECTOR ( 'NONE', #290, 1000.000000000000000 ) ;
#606 = CARTESIAN_POINT ( 'NONE',  ( -39.99999999999997868, 0.000000000000000000, -19.99999999999999645 ) ) ;
#607 = ORIENTED_EDGE ( 'NONE', *, *, #12460, .T. ) ;
#608 = DIRECTION ( 'NONE',  ( 1.000000000000000000, -0.000000000000000000, -0.000000000000000000 ) ) ;
#609 = DIRECTION ( 'NONE',  ( -1.000000000000000000, -0.000000000000000000, -0.000000000000000000 ) ) ;
#610 = DIRECTION ( 'NONE',  ( 0.000000000000000000, 0.000000000000000000, 1.000000000000000000 ) ) ;
#611 = EDGE_LOOP ( 'NONE', ( #7901, #9205, #87, #13240 ) ) ;
#612 = AXIS2_PLACEMENT_3D ( 'NONE', #4088, #1336, #229 ) ;
#613 = VECTOR ( 'NONE', #417, 1000.000000000000000 ) ;
#614 = VERTEX_POINT ( 'NONE', #13461 ) ;
#615 = EDGE_CURVE ( 'NONE', #2722, #903, #6909, .T. ) ;
#616 = ORIENTED_EDGE ( 'NONE', *, *, #4791, .F. ) ;
#617 = DIRECTION ( 'NONE',  ( -1.000000000000000000, -0.000000000000000000, -0.000000000000000000 ) ) ;
#618 = ADVANCED_FACE ( 'NONE', ( #15247 ), #15699, .T. ) ;
#619 = AXIS2_PLACEMENT_3D ( 'NONE', #348, #16146, #439 ) ;
#620 = CARTESIAN_POINT ( 'NONE',  ( 2.901926423773059760, 60.78602980190899530, 9.046021540735432964 ) ) ;
#621 = EDGE_LOOP ( 'NONE', ( #15777, #12774, #1620, #6856, #2071, #9372 ) ) ;
#622 = AXIS2_PLACEMENT_3D ( 'NONE', #13030, #1258, #10441 ) ;
#623 = AXIS2_PLACEMENT_3D ( 'NONE', #9579, #7932, #13279 ) ;
#624 = DIRECTION ( 'NONE',  ( 0.000000000000000000, 0.000000000000000000, 1.000000000000000000 ) ) ;
#625 = CARTESIAN_POINT ( 'NONE',  ( -35.00000000000000000, 8.000000000000000000, 20.99999999999999289 ) ) ;
#626 = ORIENTED_EDGE ( 'NONE', *, *, #1932, .T. ) ;
#627 = CARTESIAN_POINT ( 'NONE',  ( -26.00000000000001776, 8.000000000000000000, 33.00000000000000711 ) ) ;
#628 = APPLICATION_CONTEXT ( 'automotive_design' ) ;
#629 = DIRECTION ( 'NONE',  ( -0.000000000000000000, 1.000000000000000000, -0.000000000000000000 ) ) ;
#630 = EDGE_LOOP ( 'NONE', ( #1582, #16288, #9962, #1330, #8933 ) ) ;
#631 = AXIS2_PLACEMENT_3D ( 'NONE', #2906, #4290, #4103 ) ;
#632 = DIRECTION ( 'NONE',  ( 1.000000000000000000, -0.000000000000000000, 0.000000000000000000 ) ) ;
#633 = ORIENTED_EDGE ( 'NONE', *, *, #4265, .T. ) ;
#634 = ORIENTED_EDGE ( 'NONE', *, *, #1223, .F. ) ;
#635 = ORIENTED_EDGE ( 'NONE', *, *, #7612, .T. ) ;
#636 = ORIENTED_EDGE ( 'NONE', *, *, #1848, .F. ) ;
#637 = AXIS2_PLACEMENT_3D ( 'NONE', #5603, #12227, #10673 ) ;
#638 = ORIENTED_EDGE ( 'NONE', *, *, #2734, .T. ) ;
#639 = CYLINDRICAL_SURFACE ( 'NONE', #13237, 36.50000000000000000 ) ;
#640 = DIRECTION ( 'NONE',  ( -0.000000000000000000, -1.000000000000000000, 0.000000000000000000 ) ) ;
#641 = FACE_OUTER_BOUND ( 'NONE', #9058, .T. ) ;
#642 = VECTOR ( 'NONE', #7917, 1000.000000000000000 ) ;
#643 = AXIS2_PLACEMENT_3D ( 'NONE', #5961, #10088, #16359 ) ;
#644 = FACE_OUTER_BOUND ( 'NONE', #16902, .T. ) ;
#645 = AXIS2_PLACEMENT_3D ( 'NONE', #7793, #11580, #1282 ) ;
#646 = VECTOR ( 'NONE', #13968, 1000.000000000000000 ) ;
#647 = DIRECTION ( 'NONE',  ( 0.000000000000000000, 0.000000000000000000, -1.000000000000000000 ) ) ;
#648 = CARTESIAN_POINT ( 'NONE',  ( 19.99999999999995381, 3.000000000000000000, -39.99999999999999289 ) ) ;
#649 = DIRECTION ( 'NONE',  ( 0.000000000000000000, 0.000000000000000000, -1.000000000000000000 ) ) ;
#650 = ORIENTED_EDGE ( 'NONE', *, *, #4882, .T. ) ;
#651 = CYLINDRICAL_SURFACE ( 'NONE', #4039, 22.50000000000000000 ) ;
#652 = LINE ( 'NONE', #5966, #6353 ) ;
#653 = AXIS2_PLACEMENT_3D ( 'NONE', #5751, #11950, #5409 ) ;
#654 = FACE_OUTER_BOUND ( 'NONE', #3552, .T. ) ;
#655 = DIRECTION ( 'NONE',  ( 0.000000000000000000, 0.000000000000000000, 1.000000000000000000 ) ) ;
#657 = EDGE_LOOP ( 'NONE', ( #14248, #4305, #2695, #5890, #6096, #3804 ) ) ;
#656 = EDGE_LOOP ( 'NONE', ( #8777, #14028, #11460, #5148 ) ) ;
#658 = VECTOR ( 'NONE', #11518, 1000.000000000000000 ) ;
#659 = DIRECTION ( 'NONE',  ( 0.000000000000000000, 1.000000000000000000, 0.000000000000000000 ) ) ;
#660 = CIRCLE ( 'NONE', #10797, 5.000000000000004441 ) ;
#661 = VECTOR ( 'NONE', #10165, 1000.000000000000114 ) ;
#662 = ORIENTED_EDGE ( 'NONE', *, *, #3733, .T. ) ;
#663 = EDGE_CURVE ( 'NONE', #3748, #11164, #8302, .T. ) ;
#664 = AXIS2_PLACEMENT_3D ( 'NONE', #15934, #9420, #9333 ) ;
#665 = ADVANCED_FACE ( 'NONE', ( #1930, #12330 ), #8545, .T. ) ;
#666 = FACE_OUTER_BOUND ( 'NONE', #12649, .T. ) ;
#667 = FACE_OUTER_BOUND ( 'NONE', #15716, .T. ) ;
#668 = ORIENTED_EDGE ( 'NONE', *, *, #15780, .T. ) ;
#669 = CARTESIAN_POINT ( 'NONE',  ( 27.49999999999999645, 196.3050121726289206, -75.00000000000000000 ) ) ;
#670 = MECHANICAL_DESIGN_GEOMETRIC_PRESENTATION_REPRESENTATION (  '', ( #13291 ), #13993 ) ;
#671 = ADVANCED_FACE ( 'NONE', ( #4669 ), #16283, .F. ) ;
#672 = AXIS2_PLACEMENT_3D ( 'NONE', #2481, #2573, #15550 ) ;
#673 = DIRECTION ( 'NONE',  ( -1.000000000000000000, 1.798225651005137147E-12, 1.798225651005303603E-13 ) ) ;
#674 = ORIENTED_EDGE ( 'NONE', *, *, #12126, .F. ) ;
#675 = DIRECTION ( 'NONE',  ( 0.000000000000000000, 0.000000000000000000, -1.000000000000000000 ) ) ;
#676 = AXIS2_PLACEMENT_3D ( 'NONE', #3456, #5688, #10932 ) ;
#677 = CARTESIAN_POINT ( 'NONE',  ( -1.725642888248450024, 190.2785135797052192, 37.61614439054952186 ) ) ;
#678 = DIRECTION ( 'NONE',  ( -1.000000000000000000, -0.000000000000000000, -0.000000000000000000 ) ) ;
#679 = AXIS2_PLACEMENT_3D ( 'NONE', #15816, #4055, #2757 ) ;
#680 = CARTESIAN_POINT ( 'NONE',  ( -54.99999999999999289, 515.4878487013597805, -546.7230258972048205 ) ) ;
#681 = DIRECTION ( 'NONE',  ( -1.000000000000000000, -0.000000000000000000, -0.000000000000000000 ) ) ;
#682 = ORIENTED_EDGE ( 'NONE', *, *, #11656, .F. ) ;
#683 = FACE_OUTER_BOUND ( 'NONE', #15993, .T. ) ;
#684 =( GEOMETRIC_REPRESENTATION_CONTEXT ( 3 ) GLOBAL_UNCERTAINTY_ASSIGNED_CONTEXT ( ( #3495 ) ) GLOBAL_UNIT_ASSIGNED_CONTEXT ( ( #7732, #13159, #12899 ) ) REPRESENTATION_CONTEXT ( 'NONE', 'WORKASPACE' ) );
#685 = FACE_OUTER_BOUND ( 'NONE', #4476, .T. ) ;
#686 = EDGE_CURVE ( 'NONE', #12698, #1954, #7153, .T. ) ;
#687 = VERTEX_POINT ( 'NONE', #1861 ) ;
#688 = VECTOR ( 'NONE', #12772, 1000.000000000000000 ) ;
#689 = EDGE_CURVE ( 'NONE', #13804, #2916, #16443, .T. ) ;
#690 = ORIENTED_EDGE ( 'NONE', *, *, #1012, .F. ) ;
#691 = AXIS2_PLACEMENT_3D ( 'NONE', #9355, #14691, #13486 ) ;
#692 = CARTESIAN_POINT ( 'NONE',  ( 4.899999999999999467, -12.00000000000000000, 1.509263698769704680E-15 ) ) ;
#693 = AXIS2_PLACEMENT_3D ( 'NONE', #10981, #766, #12520 ) ;
#694 = ADVANCED_FACE ( 'NONE', ( #16525 ), #12663, .T. ) ;
#695 = EDGE_CURVE ( 'NONE', #7005, #1870, #905, .T. ) ;
#696 = EDGE_CURVE ( 'NONE', #1365, #12299, #5834, .T. ) ;
#697 = CARTESIAN_POINT ( 'NONE',  ( 49.99999999999999289, 515.4878487013597805, -546.7230258972048205 ) ) ;
#698 = ORIENTED_EDGE ( 'NONE', *, *, #4584, .F. ) ;
#699 = CARTESIAN_POINT ( 'NONE',  ( 45.00000000000000000, 523.2161522479893847, -604.2478186815853860 ) ) ;
#700 = EDGE_CURVE ( 'NONE', #3010, #49, #652, .T. ) ;
#701 = PLANE ( 'NONE',  #3805 ) ;
#702 = DIRECTION ( 'NONE',  ( 0.000000000000000000, 1.000000000000000000, 0.000000000000000000 ) ) ;
#703 = EDGE_LOOP ( 'NONE', ( #14669, #2505 ) ) ;
#704 = DIRECTION ( 'NONE',  ( 0.000000000000000000, 0.000000000000000000, 1.000000000000000000 ) ) ;
#705 = ORIENTED_EDGE ( 'NONE', *, *, #11811, .T. ) ;
#706 = EDGE_LOOP ( 'NONE', ( #5585, #7438, #14987, #3458, #12125, #5109 ) ) ;
#707 = DIRECTION ( 'NONE',  ( -0.000000000000000000, -1.000000000000000000, -0.000000000000000000 ) ) ;
#708 = VECTOR ( 'NONE', #10200, 1000.000000000000000 ) ;
#709 = SHAPE_DEFINITION_REPRESENTATION ( #16201, #16471 ) ;
#710 =( NAMED_UNIT ( * ) PLANE_ANGLE_UNIT ( ) SI_UNIT ( $, .RADIAN. ) );
#711 = CARTESIAN_POINT ( 'NONE',  ( 0.9699764831012678279, 62.84572122215210754, 9.452135968713493597 ) ) ;
#712 = EDGE_LOOP ( 'NONE', ( #7284, #9599, #2475, #11333 ) ) ;
#713 = DIRECTION ( 'NONE',  ( 1.000000000000000000, 0.000000000000000000, 0.000000000000000000 ) ) ;
#714 = EDGE_CURVE ( 'NONE', #1311, #9832, #6041, .T. ) ;
#715 = DIRECTION ( 'NONE',  ( -0.000000000000000000, 1.000000000000000000, -0.000000000000000000 ) ) ;
#716 = EDGE_CURVE ( 'NONE', #7408, #2249, #7077, .T. ) ;
#717 = VERTEX_POINT ( 'NONE', #3483 ) ;
#718 = VECTOR ( 'NONE', #5173, 1000.000000000000000 ) ;
#719 = DIRECTION ( 'NONE',  ( -1.000000000000000000, -0.000000000000000000, -0.000000000000000000 ) ) ;
#720 = ADVANCED_FACE ( 'NONE', ( #2013 ), #3235, .T. ) ;
#721 = FACE_OUTER_BOUND ( 'NONE', #15457, .T. ) ;
#722 = EDGE_LOOP ( 'NONE', ( #12294, #300, #10535, #9049 ) ) ;
#723 = LINE ( 'NONE', #880, #14088 ) ;
#724 = ORIENTED_EDGE ( 'NONE', *, *, #10666, .F. ) ;
#725 = ORIENTED_EDGE ( 'NONE', *, *, #12878, .F. ) ;
#726 = ORIENTED_EDGE ( 'NONE', *, *, #15567, .T. ) ;
#727 = SHAPE_REPRESENTATION_RELATIONSHIP ( 'NONE' , 'NONE' ,  #12962, #7706 ) ;
#728 = VECTOR ( 'NONE', #16402, 1000.000000000000000 ) ;
#729 = AXIS2_PLACEMENT_3D ( 'NONE', #5206, #10459, #2640 ) ;
#730 = ORIENTED_EDGE ( 'NONE', *, *, #13718, .F. ) ;
#731 = ORIENTED_EDGE ( 'NONE', *, *, #9384, .T. ) ;
#732 = CYLINDRICAL_SURFACE ( 'NONE', #11039, 2.500000000000002220 ) ;
#733 = CARTESIAN_POINT ( 'NONE',  ( 40.00000000000003553, -20.00000000000000000, 20.00000000000000355 ) ) ;
#734 = DIRECTION ( 'NONE',  ( -0.000000000000000000, -1.000000000000000000, -0.000000000000000000 ) ) ;
#735 = CYLINDRICAL_SURFACE ( 'NONE', #9556, 4.999999999999997335 ) ;
#736 = CARTESIAN_POINT ( 'NONE',  ( -26.00000000000002842, 3.000000000000000000, 34.00000000000000711 ) ) ;
#737 = PLANE ( 'NONE',  #10255 ) ;
#738 = TOROIDAL_SURFACE ( 'NONE', #7030, 4.695405383895982609, 9.000000000000000000 ) ;
#739 = DIRECTION ( 'NONE',  ( 1.000000000000000000, 0.000000000000000000, 0.000000000000000000 ) ) ;
#740 = VECTOR ( 'NONE', #2114, 1000.000000000000000 ) ;
#741 = FACE_BOUND ( 'NONE', #3110, .T. ) ;
#742 = VERTEX_POINT ( 'NONE', #11208 ) ;
#743 = CARTESIAN_POINT ( 'NONE',  ( 47.50000000000000000, 196.3050121726289206, -17.00000000000000000 ) ) ;
#744 = CARTESIAN_POINT ( 'NONE',  ( 46.99999999999988631, 559.9933750504617365, -546.7230258972048205 ) ) ;
#745 = LINE ( 'NONE', #2016, #3137 ) ;
#746 = CARTESIAN_POINT ( 'NONE',  ( 0.000000000000000000, 376.0487089519831443, -75.00000000000331113 ) ) ;
#748 = VERTEX_POINT ( 'NONE', #2182 ) ;
#747 = VERTEX_POINT ( 'NONE', #8726 ) ;
#749 = DIRECTION ( 'NONE',  ( -0.000000000000000000, -1.000000000000000000, -0.000000000000000000 ) ) ;
#750 = VERTEX_POINT ( 'NONE', #11127 ) ;
#751 = ADVANCED_FACE ( 'NONE', ( #9922 ), #16366, .T. ) ;
#752 = AXIS2_PLACEMENT_3D ( 'NONE', #10958, #569, #11207 ) ;
#753 = SURFACE_SIDE_STYLE ('',( #5726 ) ) ;
#754 = AXIS2_PLACEMENT_3D ( 'NONE', #13149, #16831, #1378 ) ;
#755 = FACE_OUTER_BOUND ( 'NONE', #10542, .T. ) ;
#756 = DIRECTION ( 'NONE',  ( 0.000000000000000000, 0.000000000000000000, -1.000000000000000000 ) ) ;
#757 = ORIENTED_EDGE ( 'NONE', *, *, #8896, .T. ) ;
#758 = EDGE_CURVE ( 'NONE', #14494, #13306, #7332, .T. ) ;
#759 = CARTESIAN_POINT ( 'NONE',  ( 44.99999999999998579, 515.4878487013597805, -571.7230258972048205 ) ) ;
#760 = DIRECTION ( 'NONE',  ( 1.000000000000000000, -0.000000000000000000, 0.000000000000000000 ) ) ;
#761 = ORIENTED_EDGE ( 'NONE', *, *, #4663, .F. ) ;
#762 = CARTESIAN_POINT ( 'NONE',  ( 46.99999999999988631, 473.6663340069157471, -531.5012393965008641 ) ) ;
#763 = CARTESIAN_POINT ( 'NONE',  ( 0.000000000000000000, 306.0487089519832011, -75.00000000000380851 ) ) ;
#764 = DIRECTION ( 'NONE',  ( -0.000000000000000000, -0.000000000000000000, 1.000000000000000000 ) ) ;
#765 = CIRCLE ( 'NONE', #3503, 25.00000000000002132 ) ;
#766 = DIRECTION ( 'NONE',  ( 1.000000000000000000, -0.000000000000000000, 0.000000000000000000 ) ) ;
#767 = CARTESIAN_POINT ( 'NONE',  ( 10.00000000000000000, 376.0487089519837127, -150.0000000000033538 ) ) ;
#768 = ORIENTED_EDGE ( 'NONE', *, *, #9538, .T. ) ;
#769 = DIRECTION ( 'NONE',  ( 0.000000000000000000, 0.000000000000000000, 1.000000000000000000 ) ) ;
#770 = EDGE_CURVE ( 'NONE', #8036, #5137, #1240, .T. ) ;
#771 = CARTESIAN_POINT ( 'NONE',  ( 10.00000000000000000, 309.2289037985890445, -146.8198051533984199 ) ) ;
#772 = ORIENTED_EDGE ( 'NONE', *, *, #409, .F. ) ;
#773 = DIRECTION ( 'NONE',  ( -1.000000000000000000, 0.000000000000000000, -0.000000000000000000 ) ) ;
#774 = ORIENTED_EDGE ( 'NONE', *, *, #13513, .F. ) ;
#775 = CARTESIAN_POINT ( 'NONE',  ( 0.000000000000000000, 0.000000000000000000, 35.00000000000000711 ) ) ;
#776 = DIRECTION ( 'NONE',  ( -0.000000000000000000, -0.000000000000000000, 1.000000000000000000 ) ) ;
#777 = VERTEX_POINT ( 'NONE', #14211 ) ;
#778 = CARTESIAN_POINT ( 'NONE',  ( 30.99999999999997513, 10.00000000000000000, 30.99999999999999645 ) ) ;
#779 = DIRECTION ( 'NONE',  ( -1.000000000000000000, -0.000000000000000000, -0.000000000000000000 ) ) ;
#780 = DIRECTION ( 'NONE',  ( -0.000000000000000000, -1.000000000000000000, 0.000000000000000000 ) ) ;
#781 = ORIENTED_EDGE ( 'NONE', *, *, #4458, .T. ) ;
#782 = EDGE_CURVE ( 'NONE', #3745, #10488, #8803, .T. ) ;
#783 = CARTESIAN_POINT ( 'NONE',  ( 31.00000000000001776, 10.00000000000000000, -25.99999999999999645 ) ) ;
#784 = DIRECTION ( 'NONE',  ( 0.000000000000000000, 0.000000000000000000, -1.000000000000000000 ) ) ;
#785 = VERTEX_POINT ( 'NONE', #3897 ) ;
#786 = EDGE_CURVE ( 'NONE', #9290, #5350, #6103, .T. ) ;
#787 = EDGE_LOOP ( 'NONE', ( #12595, #7263, #98, #12446 ) ) ;
#788 = LINE ( 'NONE', #3449, #2861 ) ;
#789 = AXIS2_PLACEMENT_3D ( 'NONE', #11450, #8719, #7571 ) ;
#790 = PRODUCT_CONTEXT ( 'NONE', #4781, 'mechanical' ) ;
#791 = ADVANCED_FACE ( 'NONE', ( #16939 ), #2512, .T. ) ;
#792 = DIRECTION ( 'NONE',  ( -6.123031769111888756E-17, 0.000000000000000000, -1.000000000000000000 ) ) ;
#793 = VERTEX_POINT ( 'NONE', #4923 ) ;
#794 = LINE ( 'NONE', #871, #6349 ) ;
#795 = CARTESIAN_POINT ( 'NONE',  ( 0.000000000000000000, 380.0000000000000000, 0.000000000000000000 ) ) ;
#796 = ORIENTED_EDGE ( 'NONE', *, *, #4563, .T. ) ;
#797 = CARTESIAN_POINT ( 'NONE',  ( -20.99999999999999645, 19.00000000000000000, 35.00000000000001421 ) ) ;
#798 = VECTOR ( 'NONE', #16726, 1000.000000000000000 ) ;
#799 = CARTESIAN_POINT ( 'NONE',  ( 25.99999999999997513, 10.00000000000000000, 31.00000000000003553 ) ) ;
#800 = ORIENTED_EDGE ( 'NONE', *, *, #8558, .F. ) ;
#801 = EDGE_CURVE ( 'NONE', #276, #14337, #9137, .T. ) ;
#802 = DIRECTION ( 'NONE',  ( -1.000000000000000000, -0.000000000000000000, -0.000000000000000000 ) ) ;
#803 = ORIENTED_EDGE ( 'NONE', *, *, #3451, .T. ) ;
#804 = ORIENTED_EDGE ( 'NONE', *, *, #8582, .F. ) ;
#805 = ORIENTED_EDGE ( 'NONE', *, *, #924, .T. ) ;
#806 = EDGE_CURVE ( 'NONE', #9059, #6790, #3566, .T. ) ;
#807 = ADVANCED_FACE ( 'NONE', ( #12835, #7494 ), #16771, .F. ) ;
#808 = EDGE_CURVE ( 'NONE', #12512, #9815, #9142, .T. ) ;
#809 = EDGE_CURVE ( 'NONE', #6970, #15231, #5008, .T. ) ;
#810 = EDGE_LOOP ( 'NONE', ( #14772, #2703, #1157, #4328 ) ) ;
#811 = ORIENTED_EDGE ( 'NONE', *, *, #3328, .F. ) ;
#812 = CARTESIAN_POINT ( 'NONE',  ( 1.163414460601643398E-15, 38.00000000000000711, 9.500000000000000000 ) ) ;
#813 = CARTESIAN_POINT ( 'NONE',  ( 394.0000000000001137, 341.5974953295075807, -105.4170192159777031 ) ) ;
#814 = FACE_OUTER_BOUND ( 'NONE', #2669, .T. ) ;
#815 = VECTOR ( 'NONE', #5478, 1000.000000000000000 ) ;
#816 = LINE ( 'NONE', #15240, #16408 ) ;
#817 = FACE_OUTER_BOUND ( 'NONE', #12262, .T. ) ;
#818 = LINE ( 'NONE', #565, #9425 ) ;
#819 = CARTESIAN_POINT ( 'NONE',  ( 0.000000000000000000, 3.000000000000000000, 0.000000000000000000 ) ) ;
#820 = LINE ( 'NONE', #2010, #3272 ) ;
#821 = ORIENTED_EDGE ( 'NONE', *, *, #14805, .T. ) ;
#822 = CARTESIAN_POINT ( 'NONE',  ( 30.99999999999999645, 0.000000000000000000, -25.99999999999999645 ) ) ;
#823 = DIRECTION ( 'NONE',  ( 1.000000000000000000, -0.000000000000000000, 0.000000000000000000 ) ) ;
#824 = DIRECTION ( 'NONE',  ( 0.000000000000000000, -1.000000000000000000, -1.321694076934710402E-16 ) ) ;
#826 = ORIENTED_EDGE ( 'NONE', *, *, #12976, .T. ) ;
#825 = ORIENTED_EDGE ( 'NONE', *, *, #2966, .F. ) ;
#827 = CARTESIAN_POINT ( 'NONE',  ( -34.99999999999998579, 3.000000000000000000, 21.00000000000000355 ) ) ;
#828 = PRESENTATION_LAYER_ASSIGNMENT (  '', '', ( #2462 ) ) ;
#829 = EDGE_CURVE ( 'NONE', #4632, #12051, #12754, .T. ) ;
#830 = EDGE_LOOP ( 'NONE', ( #7966, #6621, #16449, #9149 ) ) ;
#831 = CARTESIAN_POINT ( 'NONE',  ( 0.000000000000000000, 339.1725919290087745, -16.41886574335978821 ) ) ;
#832 = CIRCLE ( 'NONE', #3026, 0.7365999999986965197 ) ;
#833 = DIRECTION ( 'NONE',  ( 0.000000000000000000, -0.000000000000000000, 1.000000000000000000 ) ) ;
#834 = CARTESIAN_POINT ( 'NONE',  ( 0.000000000000000000, 339.1725919290087745, -10.68226574335978718 ) ) ;
#835 = ORIENTED_EDGE ( 'NONE', *, *, #11748, .T. ) ;
#836 = LINE ( 'NONE', #13972, #7247 ) ;
#837 = CIRCLE ( 'NONE', #10427, 4.000000000000003553 ) ;
#838 = CARTESIAN_POINT ( 'NONE',  ( 55.99999999999989342, 473.6663340069158039, -557.2494070140132862 ) ) ;
#839 = ORIENTED_EDGE ( 'NONE', *, *, #12634, .T. ) ;
#840 = CARTESIAN_POINT ( 'NONE',  ( -0.9714722756524757363, 62.84506667638981270, 9.451944983354374941 ) ) ;
#841 = AXIS2_PLACEMENT_3D ( 'NONE', #16046, #1536, #10634 ) ;
#842 = EDGE_CURVE ( 'NONE', #1983, #9375, #2545, .T. ) ;
#843 = DIRECTION ( 'NONE',  ( 0.000000000000000000, 1.000000000000000000, 0.000000000000000000 ) ) ;
#844 = CARTESIAN_POINT ( 'NONE',  ( 7.230770027832480594E-13, 214.4632308570090800, 287.5298983642209123 ) ) ;
#845 = DIRECTION ( 'NONE',  ( -1.000000000000000000, 0.000000000000000000, -0.000000000000000000 ) ) ;
#846 = CARTESIAN_POINT ( 'NONE',  ( 35.99999999999999289, 10.00000000000000000, 18.99999999999999289 ) ) ;
#847 = ORIENTED_EDGE ( 'NONE', *, *, #14322, .T. ) ;
#848 = DIRECTION ( 'NONE',  ( -1.000000000000000000, -0.000000000000000000, -0.000000000000000000 ) ) ;
#849 = AXIS2_PLACEMENT_3D ( 'NONE', #14924, #3166, #8401 ) ;
#850 = DIRECTION ( 'NONE',  ( 1.000000000000000000, 0.000000000000000000, 3.854941057726246479E-16 ) ) ;
#851 = VERTEX_POINT ( 'NONE', #1149 ) ;
#852 = DIRECTION ( 'NONE',  ( 0.000000000000000000, 0.000000000000000000, 1.000000000000000000 ) ) ;
#853 = ORIENTED_EDGE ( 'NONE', *, *, #7304, .F. ) ;
#854 = FACE_OUTER_BOUND ( 'NONE', #5998, .T. ) ;
#855 = DIRECTION ( 'NONE',  ( 1.000000000000000000, 0.000000000000000000, 0.000000000000000000 ) ) ;
#856 = VERTEX_POINT ( 'NONE', #16613 ) ;
#857 = DIRECTION ( 'NONE',  ( 0.000000000000000000, 0.000000000000000000, -1.000000000000000000 ) ) ;
#858 = DIRECTION ( 'NONE',  ( 0.000000000000000000, 0.000000000000000000, -1.000000000000000000 ) ) ;
#859 = LINE ( 'NONE', #13995, #7290 ) ;
#860 = ORIENTED_EDGE ( 'NONE', *, *, #6436, .T. ) ;
#861 = VECTOR ( 'NONE', #12744, 1000.000000000000000 ) ;
#862 = CARTESIAN_POINT ( 'NONE',  ( 37.18009836720079875, 352.3758082234937206, -75.00000000000000000 ) ) ;
#863 = DIRECTION ( 'NONE',  ( 0.000000000000000000, -0.3746065934159095168, 0.9271838545667885345 ) ) ;
#864 = EDGE_LOOP ( 'NONE', ( #15035, #505 ) ) ;
#865 = ORIENTED_EDGE ( 'NONE', *, *, #2062, .F. ) ;
#866 = LINE ( 'NONE', #15115, #3690 ) ;
#867 = APPLICATION_PROTOCOL_DEFINITION ( 'draft international standard', 'automotive_design', 1998, #1168 ) ;
#868 = PLANE ( 'NONE',  #5746 ) ;
#869 = ORIENTED_EDGE ( 'NONE', *, *, #1177, .T. ) ;
#870 = EDGE_CURVE ( 'NONE', #15712, #4694, #11591, .T. ) ;
#871 = CARTESIAN_POINT ( 'NONE',  ( 54.99999999999999289, 515.4878487013597805, -461.7230258972048205 ) ) ;
#872 = CARTESIAN_POINT ( 'NONE',  ( -40.00000000000000000, 19.00000000000000000, 25.99999999999999645 ) ) ;
#873 = EDGE_LOOP ( 'NONE', ( #5889, #10233 ) ) ;
#874 = CARTESIAN_POINT ( 'NONE',  ( -3.270000000000000462, 220.0768326692952996, 286.9685381829922903 ) ) ;
#875 = AXIS2_PLACEMENT_3D ( 'NONE', #6928, #8146, #13397 ) ;
#876 =( GEOMETRIC_REPRESENTATION_CONTEXT ( 3 ) GLOBAL_UNCERTAINTY_ASSIGNED_CONTEXT ( ( #4119 ) ) GLOBAL_UNIT_ASSIGNED_CONTEXT ( ( #5895, #12508, #9932 ) ) REPRESENTATION_CONTEXT ( 'NONE', 'WORKASPACE' ) );
#877 = LINE ( 'NONE', #9899, #2074 ) ;
#878 = ORIENTED_EDGE ( 'NONE', *, *, #6436, .F. ) ;
#879 = EDGE_CURVE ( 'NONE', #5928, #11595, #14905, .T. ) ;
#880 = CARTESIAN_POINT ( 'NONE',  ( -31.00000000000006750, 3.000000000000000000, 26.00000000000000355 ) ) ;
#881 = ORIENTED_EDGE ( 'NONE', *, *, #16843, .T. ) ;
#882 = VERTEX_POINT ( 'NONE', #7838 ) ;
#883 = AXIS2_PLACEMENT_3D ( 'NONE', #14599, #9360, #9454 ) ;
#884 = VERTEX_POINT ( 'NONE', #2349 ) ;
#885 = AXIS2_PLACEMENT_3D ( 'NONE', #15348, #2118, #15017 ) ;
#886 = VECTOR ( 'NONE', #12967, 1000.000000000000000 ) ;
#887 = ORIENTED_EDGE ( 'NONE', *, *, #3842, .F. ) ;
#888 = ORIENTED_EDGE ( 'NONE', *, *, #8243, .T. ) ;
#889 = CARTESIAN_POINT ( 'NONE',  ( 0.000000000000000000, 0.000000000000000000, 0.000000000000000000 ) ) ;
#890 = EDGE_CURVE ( 'NONE', #6948, #14037, #11627, .T. ) ;
#891 = FACE_OUTER_BOUND ( 'NONE', #5859, .T. ) ;
#892 = CARTESIAN_POINT ( 'NONE',  ( 1.163414459189985485E-15, 66.00000000000000000, 9.500000000000000000 ) ) ;
#893 = AXIS2_PLACEMENT_3D ( 'NONE', #2743, #8238, #7973 ) ;
#894 = FACE_OUTER_BOUND ( 'NONE', #3103, .T. ) ;
#895 = LINE ( 'NONE', #8636, #15441 ) ;
#896 = DIRECTION ( 'NONE',  ( 1.000000000000000000, 0.000000000000000000, 8.673617379884027583E-16 ) ) ;
#897 = EDGE_CURVE ( 'NONE', #9574, #11859, #6282, .T. ) ;
#898 = ADVANCED_FACE ( 'NONE', ( #9051 ), #14288, .F. ) ;
#899 = DIRECTION ( 'NONE',  ( -1.000000000000000000, -0.000000000000000000, -0.000000000000000000 ) ) ;
#900 = EDGE_CURVE ( 'NONE', #13213, #10460, #15909, .T. ) ;
#901 = FACE_OUTER_BOUND ( 'NONE', #228, .T. ) ;
#902 = AXIS2_PLACEMENT_3D ( 'NONE', #9006, #9176, #73 ) ;
#903 = VERTEX_POINT ( 'NONE', #9572 ) ;
#904 = DIRECTION ( 'NONE',  ( 0.000000000000000000, 0.000000000000000000, -1.000000000000000000 ) ) ;
#905 = LINE ( 'NONE', #6125, #13249 ) ;
#906 = CARTESIAN_POINT ( 'NONE',  ( -270.0000000000000000, 0.000000000000000000, 0.000000000000000000 ) ) ;
#908 = ORIENTED_EDGE ( 'NONE', *, *, #6783, .F. ) ;
#907 = ORIENTED_EDGE ( 'NONE', *, *, #3318, .F. ) ;
#909 = AXIS2_PLACEMENT_3D ( 'NONE', #13908, #2132, #7360 ) ;
#910 = DIRECTION ( 'NONE',  ( 0.000000000000000000, 1.000000000000000000, 0.000000000000000000 ) ) ;
#911 = DIRECTION ( 'NONE',  ( 1.000000000000000000, 0.000000000000000000, 0.000000000000000000 ) ) ;
#912 = TOROIDAL_SURFACE ( 'NONE', #10781, 4.695405383895982609, 9.000000000000000000 ) ;
#913 = AXIS2_PLACEMENT_3D ( 'NONE', #4189, #11920, #14675 ) ;
#914 = DIRECTION ( 'NONE',  ( 1.000000000000000000, 0.000000000000000000, -0.000000000000000000 ) ) ;
#915 = DIRECTION ( 'NONE',  ( 0.000000000000000000, 0.000000000000000000, -1.000000000000000000 ) ) ;
#916 = ORIENTED_EDGE ( 'NONE', *, *, #6292, .T. ) ;
#917 = DIRECTION ( 'NONE',  ( 0.000000000000000000, -1.224646799147352714E-16, 1.000000000000000000 ) ) ;
#918 = ADVANCED_FACE ( 'NONE', ( #13526 ), #5515, .T. ) ;
#919 = AXIS2_PLACEMENT_3D ( 'NONE', #1143, #10501, #11876 ) ;
#920 = ADVANCED_FACE ( 'NONE', ( #10597 ), #4151, .F. ) ;
#921 = CARTESIAN_POINT ( 'NONE',  ( 54.99999999999999289, 459.5014304922595443, -192.4166442068759579 ) ) ;
#922 = ORIENTED_EDGE ( 'NONE', *, *, #8662, .T. ) ;
#923 = DIRECTION ( 'NONE',  ( -1.000000000000000000, 0.000000000000000000, -0.000000000000000000 ) ) ;
#924 = EDGE_CURVE ( 'NONE', #11643, #9884, #15834, .T. ) ;
#925 = CARTESIAN_POINT ( 'NONE',  ( 0.7365999999999708336, 189.4306931408914920, 37.53315213583260856 ) ) ;
#926 = FACE_OUTER_BOUND ( 'NONE', #7504, .T. ) ;
#927 = VECTOR ( 'NONE', #2862, 1000.000000000000000 ) ;
#928 = DIRECTION ( 'NONE',  ( 0.000000000000000000, -1.000000000000000000, 0.000000000000000000 ) ) ;
#929 = AXIS2_PLACEMENT_3D ( 'NONE', #3641, #4997, #16603 ) ;
#930 = CARTESIAN_POINT ( 'NONE',  ( 35.00000000000000711, 8.000000000000000000, 35.00000000000000711 ) ) ;
#931 = ORIENTED_EDGE ( 'NONE', *, *, #10790, .F. ) ;
#932 = CARTESIAN_POINT ( 'NONE',  ( -37.00000000000000711, 10.00000000000000000, -23.00000000000000000 ) ) ;
#933 = VECTOR ( 'NONE', #1683, 1000.000000000000000 ) ;
#934 = VECTOR ( 'NONE', #6013, 1000.000000000000000 ) ;
#935 = LINE ( 'NONE', #11070, #3557 ) ;
#936 = DIRECTION ( 'NONE',  ( 0.000000000000000000, 0.000000000000000000, -1.000000000000000000 ) ) ;
#937 = CIRCLE ( 'NONE', #10530, 3.300000000000000711 ) ;
#938 = ORIENTED_EDGE ( 'NONE', *, *, #13325, .F. ) ;
#939 = VECTOR ( 'NONE', #7634, 1000.000000000000000 ) ;
#940 = DIRECTION ( 'NONE',  ( -0.000000000000000000, -1.000000000000000000, 0.000000000000000000 ) ) ;
#941 = CARTESIAN_POINT ( 'NONE',  ( 35.99999999999999289, 10.00000000000000000, 21.99999999999999645 ) ) ;
#942 = ORIENTED_EDGE ( 'NONE', *, *, #7282, .T. ) ;
#943 = CARTESIAN_POINT ( 'NONE',  ( 45.00000000000000000, 493.2350855268092573, -598.9613477082210693 ) ) ;
#944 = AXIS2_PLACEMENT_3D ( 'NONE', #1343, #6564, #11817 ) ;
#945 = FACE_OUTER_BOUND ( 'NONE', #12335, .T. ) ;
#946 = DIRECTION ( 'NONE',  ( -0.000000000000000000, -1.000000000000000000, -0.000000000000000000 ) ) ;
#947 = ORIENTED_EDGE ( 'NONE', *, *, #7819, .F. ) ;
#948 = DIRECTION ( 'NONE',  ( -1.000000000000000000, 0.000000000000000000, 0.000000000000000000 ) ) ;
#949 = DIRECTION ( 'NONE',  ( 0.000000000000000000, 0.000000000000000000, -1.000000000000000000 ) ) ;
#950 = LINE ( 'NONE', #2313, #2276 ) ;
#951 = ORIENTED_EDGE ( 'NONE', *, *, #9601, .T. ) ;
#952 = CARTESIAN_POINT ( 'NONE',  ( 6.117449311278481738E-17, 277.8092731128509740, -44.71049682360898458 ) ) ;
#953 = CIRCLE ( 'NONE', #11923, 9.500000000000000000 ) ;
#954 =( REPRESENTATION_RELATIONSHIP ('NONE','NONE', #15277, #1329 ) REPRESENTATION_RELATIONSHIP_WITH_TRANSFORMATION ( #3532 )SHAPE_REPRESENTATION_RELATIONSHIP( ) );
#955 =( LENGTH_UNIT ( ) NAMED_UNIT ( * ) SI_UNIT ( .MILLI., .METRE. ) );
#956 = VECTOR ( 'NONE', #13594, 1000.000000000000000 ) ;
#957 = EDGE_CURVE ( 'NONE', #5265, #14388, #10680, .T. ) ;
#958 = DIRECTION ( 'NONE',  ( 1.000000000000000000, 0.000000000000000000, 0.000000000000000000 ) ) ;
#959 = ORIENTED_EDGE ( 'NONE', *, *, #10890, .T. ) ;
#960 = DIRECTION ( 'NONE',  ( -0.000000000000000000, -1.000000000000000000, -0.000000000000000000 ) ) ;
#961 = DIRECTION ( 'NONE',  ( 0.000000000000000000, 0.000000000000000000, 1.000000000000000000 ) ) ;
#962 = ADVANCED_FACE ( 'NONE', ( #9310 ), #15745, .F. ) ;
#963 = VERTEX_POINT ( 'NONE', #8006 ) ;
#964 = FACE_OUTER_BOUND ( 'NONE', #3481, .T. ) ;
#965 = LINE ( 'NONE', #11513, #1254 ) ;
#966 = ORIENTED_EDGE ( 'NONE', *, *, #15704, .T. ) ;
#967 = CIRCLE ( 'NONE', #2876, 3.300000000000000711 ) ;
#968 = CYLINDRICAL_SURFACE ( 'NONE', #6957, 14.59999999999999964 ) ;
#969 = VECTOR ( 'NONE', #13811, 1000.000000000000000 ) ;
#970 = ORIENTED_EDGE ( 'NONE', *, *, #1566, .F. ) ;
#971 = VERTEX_POINT ( 'NONE', #14636 ) ;
#972 = PRODUCT_RELATED_PRODUCT_CATEGORY ( 'part', '', ( #16847 ) ) ;
#973 = ORIENTED_EDGE ( 'NONE', *, *, #6528, .F. ) ;
#974 = VERTEX_POINT ( 'NONE', #7921 ) ;
#975 = ADVANCED_FACE ( 'NONE', ( #9394 ), #10508, .F. ) ;
#976 = VERTEX_POINT ( 'NONE', #4338 ) ;
#977 = AXIS2_PLACEMENT_3D ( 'NONE', #10796, #8211, #64 ) ;
#978 = DIRECTION ( 'NONE',  ( -0.000000000000000000, -1.000000000000000000, -0.000000000000000000 ) ) ;
#979 = FACE_OUTER_BOUND ( 'NONE', #10930, .T. ) ;
#980 = FACE_OUTER_BOUND ( 'NONE', #7929, .T. ) ;
#981 = LINE ( 'NONE', #8797, #5291 ) ;
#982 = DIRECTION ( 'NONE',  ( 0.000000000000000000, -0.9848077530122086864, 0.1736481776669273613 ) ) ;
#983 = LINE ( 'NONE', #12831, #15918 ) ;
#984 = FACE_BOUND ( 'NONE', #6638, .T. ) ;
#985 = VERTEX_POINT ( 'NONE', #16002 ) ;
#986 = DIRECTION ( 'NONE',  ( 1.000000000000000000, 0.000000000000000000, 0.000000000000000000 ) ) ;
#987 = DIRECTION ( 'NONE',  ( 0.000000000000000000, 0.000000000000000000, -1.000000000000000000 ) ) ;
#988 = EDGE_LOOP ( 'NONE', ( #15839, #11298, #10408, #266 ) ) ;
#989 = TOROIDAL_SURFACE ( 'NONE', #7022, 22.46376988133006236, 4.000164074322307250 ) ;
#990 = ADVANCED_FACE ( 'NONE', ( #10855 ), #912, .T. ) ;
#991 = AXIS2_PLACEMENT_3D ( 'NONE', #12113, #186, #5407 ) ;
#992 = ADVANCED_FACE ( 'NONE', ( #10764 ), #3994, .T. ) ;
#993 = CARTESIAN_POINT ( 'NONE',  ( -55.99999999999988631, 0.000000000000000000, 0.000000000000000000 ) ) ;
#995 = ORIENTED_EDGE ( 'NONE', *, *, #8869, .T. ) ;
#994 = EDGE_LOOP ( 'NONE', ( #9054, #6956, #636, #13363 ) ) ;
#996 = CARTESIAN_POINT ( 'NONE',  ( 46.99999999999988631, 473.6663340069157471, -545.1966447803968094 ) ) ;
#997 = VERTEX_POINT ( 'NONE', #8272 ) ;
#998 = EDGE_CURVE ( 'NONE', #9092, #5074, #1584, .T. ) ;
#999 = CARTESIAN_POINT ( 'NONE',  ( 39.41161623800082481, 323.9612906317821057, 0.000000000000000000 ) ) ;
#1000 = EDGE_CURVE ( 'NONE', #13474, #21, #3113, .T. ) ;
#1001 = CARTESIAN_POINT ( 'NONE',  ( 394.0000000000001137, 339.1725919290084335, -111.4188657433597456 ) ) ;
#1002 = CARTESIAN_POINT ( 'NONE',  ( -26.00000000000002842, 3.000000000000000000, -31.00000000000003197 ) ) ;
#1003 = VECTOR ( 'NONE', #9329, 1000.000000000000000 ) ;
#1004 = VERTEX_POINT ( 'NONE', #14470 ) ;
#1005 = VECTOR ( 'NONE', #776, 1000.000000000000000 ) ;
#1006 = PLANE ( 'NONE',  #2046 ) ;
#1007 = DIRECTION ( 'NONE',  ( -0.000000000000000000, -1.000000000000000000, 0.000000000000000000 ) ) ;
#1008 = ORIENTED_EDGE ( 'NONE', *, *, #4654, .T. ) ;
#1009 = DIRECTION ( 'NONE',  ( 1.000000000000000000, 0.000000000000000000, 0.000000000000000000 ) ) ;
#1010 = LINE ( 'NONE', #3831, #8134 ) ;
#1011 = CARTESIAN_POINT ( 'NONE',  ( 39.75350601975127063, 301.2117639810886089, -6.736600000000000144 ) ) ;
#1012 = EDGE_CURVE ( 'NONE', #2613, #16499, #12145, .T. ) ;
#1013 = CYLINDRICAL_SURFACE ( 'NONE', #16824, 7.500000000000000000 ) ;
#1014 = CARTESIAN_POINT ( 'NONE',  ( 46.99999999999988631, 523.2161522479893847, -590.5524132976893270 ) ) ;
#1015 = ORIENTED_EDGE ( 'NONE', *, *, #13635, .F. ) ;
#1016 = AXIS2_PLACEMENT_3D ( 'NONE', #3650, #15408, #904 ) ;
#1017 = CARTESIAN_POINT ( 'NONE',  ( 39.72345254347677468, 303.2115381654813859, 0.000000000000000000 ) ) ;
#1018 = TOROIDAL_SURFACE ( 'NONE', #16362, 4.695405383895982609, 9.000000000000000000 ) ;
#1019 = EDGE_CURVE ( 'NONE', #14941, #1746, #34, .T. ) ;
#1020 = ADVANCED_FACE ( 'NONE', ( #13178 ), #1403, .T. ) ;
#1021 = EDGE_CURVE ( 'NONE', #2369, #7414, #12312, .T. ) ;
#1022 = FACE_OUTER_BOUND ( 'NONE', #2431, .T. ) ;
#1023 = ADVANCED_FACE ( 'NONE', ( #2223 ), #1910, .T. ) ;
#1024 = CARTESIAN_POINT ( 'NONE',  ( -20.99999999999999645, 8.000000000000000000, -31.00000000000003908 ) ) ;
#1025 = ORIENTED_EDGE ( 'NONE', *, *, #8889, .T. ) ;
#1026 = DIRECTION ( 'NONE',  ( -1.000000000000000000, 0.000000000000000000, 0.000000000000000000 ) ) ;
#1027 = AXIS2_PLACEMENT_3D ( 'NONE', #12059, #2774, #16001 ) ;
#1028 = CARTESIAN_POINT ( 'NONE',  ( 21.99999999999998224, 8.000000000000000000, -35.99999999999999289 ) ) ;
#1029 = EDGE_LOOP ( 'NONE', ( #11785, #8696, #16101, #13084 ) ) ;
#1030 = DIRECTION ( 'NONE',  ( -0.000000000000000000, 1.000000000000000000, -0.000000000000000000 ) ) ;
#1031 = LINE ( 'NONE', #2469, #4368 ) ;
#1032 = FACE_OUTER_BOUND ( 'NONE', #15005, .T. ) ;
#1033 = ORIENTED_EDGE ( 'NONE', *, *, #15874, .T. ) ;
#1034 = DIRECTION ( 'NONE',  ( -0.000000000000000000, 1.000000000000000000, -0.000000000000000000 ) ) ;
#1035 = PLANE ( 'NONE',  #1461 ) ;
#1036 = ORIENTED_EDGE ( 'NONE', *, *, #10885, .F. ) ;
#1037 = FACE_OUTER_BOUND ( 'NONE', #656, .T. ) ;
#1038 = AXIS2_PLACEMENT_3D ( 'NONE', #4074, #10596, #10679 ) ;
#1039 = EDGE_CURVE ( 'NONE', #7998, #1155, #14979, .T. ) ;
#1040 = EDGE_LOOP ( 'NONE', ( #5659, #15885, #8082, #11990 ) ) ;
#1041 = DIRECTION ( 'NONE',  ( 1.000000000000000000, -0.000000000000000000, -0.000000000000000000 ) ) ;
#1042 = DIRECTION ( 'NONE',  ( -0.000000000000000000, -1.000000000000000000, -0.000000000000000000 ) ) ;
#1043 = CARTESIAN_POINT ( 'NONE',  ( 46.99999999999988631, 549.5810598491749488, -575.3306267969850296 ) ) ;
#1044 = VERTEX_POINT ( 'NONE', #13614 ) ;
#1045 = DIRECTION ( 'NONE',  ( -1.000000000000000000, -0.000000000000000000, 0.000000000000000000 ) ) ;
#1046 = CARTESIAN_POINT ( 'NONE',  ( 1.163414459189985485E-15, 10.00000000000000000, 9.500000000000000000 ) ) ;
#1047 = ORIENTED_EDGE ( 'NONE', *, *, #5725, .F. ) ;
#1048 = CIRCLE ( 'NONE', #7066, 13.69540538389598083 ) ;
#1049 = DIRECTION ( 'NONE',  ( -1.597771622610217359E-16, 1.000000000000000000, 0.000000000000000000 ) ) ;
#1050 = ORIENTED_EDGE ( 'NONE', *, *, #7090, .T. ) ;
#1051 = ORIENTED_EDGE ( 'NONE', *, *, #8374, .T. ) ;
#1052 = CARTESIAN_POINT ( 'NONE',  ( -31.81980515339462912, 11.00000000000000000, 35.11980515339465825 ) ) ;
#1053 = ORIENTED_EDGE ( 'NONE', *, *, #15007, .T. ) ;
#1054 = EDGE_LOOP ( 'NONE', ( #15987, #9860, #7839, #7816 ) ) ;
#1055 = ORIENTED_EDGE ( 'NONE', *, *, #1441, .F. ) ;
#1056 = AXIS2_PLACEMENT_3D ( 'NONE', #4958, #3776, #3522 ) ;
#1057 = CARTESIAN_POINT ( 'NONE',  ( 0.000000000000000000, 234.3157724647196289, -17.15546574335979813 ) ) ;
#1058 = CARTESIAN_POINT ( 'NONE',  ( -3.269999999998713491, 260.4765148507196386, 287.1312267635918829 ) ) ;
#1059 = DIRECTION ( 'NONE',  ( 0.000000000000000000, 0.000000000000000000, 1.000000000000000000 ) ) ;
#1060 = PLANE ( 'NONE',  #1731 ) ;
#1061 = DIRECTION ( 'NONE',  ( -1.000000000000000000, 0.000000000000000000, 0.000000000000000000 ) ) ;
#1062 = DIRECTION ( 'NONE',  ( 0.000000000000000000, 0.000000000000000000, 1.000000000000000000 ) ) ;
#1063 = CARTESIAN_POINT ( 'NONE',  ( 31.81980515339464333, 0.000000000000000000, 35.11980515339463693 ) ) ;
#1064 = ORIENTED_EDGE ( 'NONE', *, *, #842, .F. ) ;
#1065 = DIRECTION ( 'NONE',  ( 0.000000000000000000, -0.000000000000000000, -1.000000000000000000 ) ) ;
#1066 = DIRECTION ( 'NONE',  ( 0.000000000000000000, 1.000000000000000000, 1.321694076934710402E-16 ) ) ;
#1067 = ORIENTED_EDGE ( 'NONE', *, *, #14128, .T. ) ;
#1068 = FACE_OUTER_BOUND ( 'NONE', #12225, .T. ) ;
#1070 = ORIENTED_EDGE ( 'NONE', *, *, #15795, .F. ) ;
#1069 = VERTEX_POINT ( 'NONE', #1840 ) ;
#1071 = APPLICATION_CONTEXT ( 'automotive_design' ) ;
#1072 = FACE_OUTER_BOUND ( 'NONE', #11758, .T. ) ;
#1073 = VERTEX_POINT ( 'NONE', #15296 ) ;
#1074 = VECTOR ( 'NONE', #899, 1000.000000000000000 ) ;
#1075 = CARTESIAN_POINT ( 'NONE',  ( 0.000000000000000000, 8.000000000000000000, 0.000000000000000000 ) ) ;
#1076 = CARTESIAN_POINT ( 'NONE',  ( 0.7366000000000088033, 192.7170024689980323, 37.20452120302199006 ) ) ;
#1077 = LINE ( 'NONE', #1250, #94 ) ;
#1078 = ORIENTED_EDGE ( 'NONE', *, *, #11191, .F. ) ;
#1079 = ADVANCED_FACE ( 'NONE', ( #551 ), #6362, .T. ) ;
#1080 = PRODUCT ( 'Part9', 'Part9', '', ( #1648 ) ) ;
#1081 = LINE ( 'NONE', #10437, #5575 ) ;
#1082 = VERTEX_POINT ( 'NONE', #3527 ) ;
#1083 = CARTESIAN_POINT ( 'NONE',  ( 0.000000000000000000, 0.000000000000000000, 0.000000000000000000 ) ) ;
#1084 = FACE_OUTER_BOUND ( 'NONE', #9002, .T. ) ;
#1085 = CARTESIAN_POINT ( 'NONE',  ( 23.00000000000000711, 68.00000000000000000, -36.99999999999999289 ) ) ;
#1086 = EDGE_CURVE ( 'NONE', #4609, #9484, #7058, .T. ) ;
#1087 = EDGE_CURVE ( 'NONE', #155, #13073, #8039, .T. ) ;
#1088 = CARTESIAN_POINT ( 'NONE',  ( 46.99999999999988631, 549.5810598491746077, -531.8108303813202156 ) ) ;
#1089 = CARTESIAN_POINT ( 'NONE',  ( 394.0000000000001137, 240.7889724647196488, -16.41886574335980242 ) ) ;
#1090 = ORIENTED_EDGE ( 'NONE', *, *, #14104, .F. ) ;
#1091 = PLANE ( 'NONE',  #3181 ) ;
#1092 = DIRECTION ( 'NONE',  ( 0.000000000000000000, 0.000000000000000000, -1.000000000000000000 ) ) ;
#1093 = DIRECTION ( 'NONE',  ( 0.000000000000000000, 0.000000000000000000, -1.000000000000000000 ) ) ;
#1094 = VECTOR ( 'NONE', #412, 1000.000000000000000 ) ;
#1095 = EDGE_LOOP ( 'NONE', ( #12425, #5383 ) ) ;
#1096 = ADVANCED_FACE ( 'NONE', ( #3607 ), #16731, .F. ) ;
#1097 = VECTOR ( 'NONE', #4107, 1000.000000000000000 ) ;
#1098 = LINE ( 'NONE', #6161, #11861 ) ;
#1099 = DIRECTION ( 'NONE',  ( -1.000000000000000000, 0.000000000000000000, 0.000000000000000000 ) ) ;
#1100 = ORIENTED_EDGE ( 'NONE', *, *, #5272, .T. ) ;
#1101 = FACE_OUTER_BOUND ( 'NONE', #11342, .T. ) ;
#1102 = EDGE_CURVE ( 'NONE', #14019, #15661, #53, .T. ) ;
#1103 = CARTESIAN_POINT ( 'NONE',  ( -45.00000000000000000, 515.4878487013597805, -546.7230258972048205 ) ) ;
#1104 = DIRECTION ( 'NONE',  ( 0.000000000000000000, 0.000000000000000000, -1.000000000000000000 ) ) ;
#1105 = DIRECTION ( 'NONE',  ( 0.000000000000000000, 0.000000000000000000, 1.000000000000000000 ) ) ;
#1106 = EDGE_CURVE ( 'NONE', #14016, #14542, #950, .T. ) ;
#1107 = EDGE_CURVE ( 'NONE', #4162, #11680, #14076, .T. ) ;
#1108 = EDGE_CURVE ( 'NONE', #11237, #10016, #3215, .T. ) ;
#1109 = ADVANCED_FACE ( 'NONE', ( #10942 ), #1035, .T. ) ;
#1110 = CARTESIAN_POINT ( 'NONE',  ( 25.99999999999997868, 10.00000000000000000, 40.00000000000000711 ) ) ;
#1111 = CARTESIAN_POINT ( 'NONE',  ( 449.9999999999998295, 75.00000000000001421, 3.000000000000000000 ) ) ;
#1112 = CARTESIAN_POINT ( 'NONE',  ( 435.7731165870194445, 329.6061121441327941, -6.736600000000000144 ) ) ;
#1113 = EDGE_LOOP ( 'NONE', ( #9302, #15416, #3319, #4631 ) ) ;
#1114 = AXIS2_PLACEMENT_3D ( 'NONE', #5436, #4250, #9490 ) ;
#1115 = PLANE ( 'NONE',  #5608 ) ;
#1116 = ITEM_DEFINED_TRANSFORMATION ( 'NONE', 'NONE', #11922,  #1488 ) ;
#1117 = VECTOR ( 'NONE', #2312, 1000.000000000000000 ) ;
#1118 = ORIENTED_EDGE ( 'NONE', *, *, #1108, .F. ) ;
#1119 = DIRECTION ( 'NONE',  ( 0.000000000000000000, -0.000000000000000000, -1.000000000000000000 ) ) ;
#1120 = CYLINDRICAL_SURFACE ( 'NONE', #3661, 20.75209553982835331 ) ;
#1121 = AXIS2_PLACEMENT_3D ( 'NONE', #5551, #10800, #4365 ) ;
#1122 = CYLINDRICAL_SURFACE ( 'NONE', #13462, 4.999999999999997335 ) ;
#1123 = ORIENTED_EDGE ( 'NONE', *, *, #16120, .T. ) ;
#1124 = DIRECTION ( 'NONE',  ( -1.000000000000000000, -0.000000000000000000, -0.000000000000000000 ) ) ;
#1125 = ADVANCED_FACE ( 'NONE', ( #16655 ), #470, .F. ) ;
#1126 = LINE ( 'NONE', #10572, #5684 ) ;
#1127 = ORIENTED_EDGE ( 'NONE', *, *, #598, .T. ) ;
#1128 = EDGE_CURVE ( 'NONE', #13804, #10865, #16173, .T. ) ;
#1129 = ADVANCED_FACE ( 'NONE', ( #3135 ), #8370, .F. ) ;
#1130 = FACE_OUTER_BOUND ( 'NONE', #6538, .T. ) ;
#1131 = EDGE_LOOP ( 'NONE', ( #93, #3115, #16155, #1575 ) ) ;
#1132 = VERTEX_POINT ( 'NONE', #1112 ) ;
#1133 = DIRECTION ( 'NONE',  ( -1.000000000000000000, -0.000000000000000000, -0.000000000000000000 ) ) ;
#1134 = ORIENTED_EDGE ( 'NONE', *, *, #9509, .F. ) ;
#1135 = VECTOR ( 'NONE', #13366, 1000.000000000000000 ) ;
#1136 = ORIENTED_EDGE ( 'NONE', *, *, #14537, .T. ) ;
#1137 = VERTEX_POINT ( 'NONE', #2566 ) ;
#1138 = CLOSED_SHELL ( 'NONE', ( #15165, #6252, #9269, #4888, #3658, #807, #7631, #15966, #10966, #11049, #10661, #15869, #8338, #5630, #9841, #4327, #3632, #5285, #1796, #13193 ) ) ;
#1139 = AXIS2_PLACEMENT_3D ( 'NONE', #14241, #6310, #11563 ) ;
#1140 = CARTESIAN_POINT ( 'NONE',  ( -46.99999999999988631, 549.5810598491746077, -518.1154249974242703 ) ) ;
#1141 = DIRECTION ( 'NONE',  ( 0.000000000000000000, -1.000000000000000000, 0.000000000000000000 ) ) ;
#1142 = VERTEX_POINT ( 'NONE', #4034 ) ;
#1143 = CARTESIAN_POINT ( 'NONE',  ( 0.000000000000000000, 0.000000000000000000, 0.000000000000000000 ) ) ;
#1144 = CARTESIAN_POINT ( 'NONE',  ( 1.050000000000000044, -17.52499999999999858, -2.146193515505736390E-15 ) ) ;
#1145 = VECTOR ( 'NONE', #9983, 1000.000000000000000 ) ;
#1146 = DIRECTION ( 'NONE',  ( 0.000000000000000000, 1.000000000000000000, 0.000000000000000000 ) ) ;
#1147 = ORIENTED_EDGE ( 'NONE', *, *, #9402, .F. ) ;
#1148 = DIRECTION ( 'NONE',  ( -1.000000000000000000, -0.000000000000000000, -0.000000000000000000 ) ) ;
#1149 = CARTESIAN_POINT ( 'NONE',  ( -10.00000000000000000, 0.000000000000000000, -5.268482129199949959 ) ) ;
#1150 = VERTEX_POINT ( 'NONE', #4110 ) ;
#1151 = AXIS2_PLACEMENT_3D ( 'NONE', #11728, #1512, #13284 ) ;
#1152 = DIRECTION ( 'NONE',  ( 0.000000000000000000, 0.000000000000000000, -1.000000000000000000 ) ) ;
#1153 = ORIENTED_EDGE ( 'NONE', *, *, #1515, .F. ) ;
#1154 = DIRECTION ( 'NONE',  ( 0.000000000000000000, 0.000000000000000000, -1.000000000000000000 ) ) ;
#1155 = VERTEX_POINT ( 'NONE', #7881 ) ;
#1156 = VECTOR ( 'NONE', #14183, 1000.000000000000000 ) ;
#1157 = ORIENTED_EDGE ( 'NONE', *, *, #12746, .F. ) ;
#1158 = CARTESIAN_POINT ( 'NONE',  ( -40.00000000000000711, 6.000000000000000000, -18.00000000000000355 ) ) ;
#1159 = DIRECTION ( 'NONE',  ( 0.000000000000000000, 1.000000000000000000, 0.000000000000000000 ) ) ;
#1160 = DIRECTION ( 'NONE',  ( 0.000000000000000000, 0.000000000000000000, -1.000000000000000000 ) ) ;
#1161 = AXIS2_PLACEMENT_3D ( 'NONE', #3082, #13571, #9788 ) ;
#1162 = EDGE_LOOP ( 'NONE', ( #6373, #8256, #3553, #16098, #13335, #4560, #4416, #2032, #9926, #13252, #5328, #6594, #4833, #1994, #6733, #6071, #7894, #4053, #11863, #14292, #4454, #11780, #768, #13512, #14863, #62, #11534, #6786 ) ) ;
#1163 = CARTESIAN_POINT ( 'NONE',  ( 17.00000000000000711, 380.0000000000000000, -17.00000000000000355 ) ) ;
#1164 = VECTOR ( 'NONE', #10012, 1000.000000000000000 ) ;
#1165 = VECTOR ( 'NONE', #6571, 1000.000000000000000 ) ;
#1166 = CARTESIAN_POINT ( 'NONE',  ( -33.00000000000000000, 8.000000000000000000, -26.00000000000000355 ) ) ;
#1167 = PLANE ( 'NONE',  #9332 ) ;
#1168 = APPLICATION_CONTEXT ( 'automotive_design' ) ;
#1169 = CARTESIAN_POINT ( 'NONE',  ( 0.05133912195990903565, 193.2999246972671870, 37.48177757739162530 ) ) ;
#1170 = CARTESIAN_POINT ( 'NONE',  ( 35.99999999999999289, 8.000000000000000000, 18.99999999999999289 ) ) ;
#1171 = AXIS2_PLACEMENT_3D ( 'NONE', #9262, #7871, #12008 ) ;
#1172 = DIRECTION ( 'NONE',  ( 0.000000000000000000, -0.000000000000000000, 1.000000000000000000 ) ) ;
#1173 = CARTESIAN_POINT ( 'NONE',  ( 1.286622718088565479E-12, 285.4366476906530465, 37.52989836422118941 ) ) ;
#1175 = EDGE_LOOP ( 'NONE', ( #12902, #13410, #14916, #4640, #5689, #1663, #8940, #6414 ) ) ;
#1174 = ORIENTED_EDGE ( 'NONE', *, *, #8965, .F. ) ;
#1176 = DIRECTION ( 'NONE',  ( 0.000000000000000000, 0.000000000000000000, -1.000000000000000000 ) ) ;
#1177 = EDGE_CURVE ( 'NONE', #10479, #13438, #7704, .T. ) ;
#1178 = AXIS2_PLACEMENT_3D ( 'NONE', #16090, #14727, #5434 ) ;
#1179 = VECTOR ( 'NONE', #7670, 1000.000000000000114 ) ;
#1180 = CARTESIAN_POINT ( 'NONE',  ( 23.00000000000000711, 68.00000000000000000, -31.00000000000002487 ) ) ;
#1181 = DIRECTION ( 'NONE',  ( 0.000000000000000000, 0.000000000000000000, -1.000000000000000000 ) ) ;
#1182 = VECTOR ( 'NONE', #9131, 1000.000000000000000 ) ;
#1183 = EDGE_CURVE ( 'NONE', #8690, #14834, #11730, .T. ) ;
#1184 = ORIENTED_EDGE ( 'NONE', *, *, #14322, .F. ) ;
#1185 = DIRECTION ( 'NONE',  ( -1.000000000000000000, -0.000000000000000000, -0.000000000000000000 ) ) ;
#1186 = AXIS2_PLACEMENT_3D ( 'NONE', #8388, #1774, #230 ) ;
#1187 = DIRECTION ( 'NONE',  ( 0.000000000000000000, 0.000000000000000000, -1.000000000000000000 ) ) ;
#1188 = VERTEX_POINT ( 'NONE', #12959 ) ;
#1189 = CARTESIAN_POINT ( 'NONE',  ( 394.0000000000001137, 451.4647406485092915, -149.8062676851188257 ) ) ;
#1190 = AXIS2_PLACEMENT_3D ( 'NONE', #15516, #3825, #7593 ) ;
#1191 = CARTESIAN_POINT ( 'NONE',  ( -35.00000000000000000, 19.00000000000000000, 20.99999999999999289 ) ) ;
#1192 = CARTESIAN_POINT ( 'NONE',  ( -26.00000000000002132, 10.00000000000000000, 40.00000000000000711 ) ) ;
#1193 = LINE ( 'NONE', #5134, #4445 ) ;
#1194 = DIRECTION ( 'NONE',  ( 0.000000000000000000, 1.000000000000000000, 0.000000000000000000 ) ) ;
#1195 = LINE ( 'NONE', #6498, #1974 ) ;
#1196 = VERTEX_POINT ( 'NONE', #14423 ) ;
#1197 = CIRCLE ( 'NONE', #10802, 15.00000000000000000 ) ;
#1198 = DIRECTION ( 'NONE',  ( -1.000000000000000000, -0.000000000000000000, 0.000000000000000000 ) ) ;
#1199 = EDGE_CURVE ( 'NONE', #13085, #5980, #15985, .T. ) ;
#1200 = EDGE_CURVE ( 'NONE', #8036, #5519, #15702, .T. ) ;
#1201 = ITEM_DEFINED_TRANSFORMATION ( 'NONE', 'NONE', #2589,  #1488 ) ;
#1202 = AXIS2_PLACEMENT_3D ( 'NONE', #15389, #8864, #1049 ) ;
#1203 = CIRCLE ( 'NONE', #11075, 5.268482129199949959 ) ;
#1204 = EDGE_CURVE ( 'NONE', #6942, #10732, #11840, .T. ) ;
#1205 = CARTESIAN_POINT ( 'NONE',  ( 29.68009836720079875, 275.4439001176564830, -75.00000000000000000 ) ) ;
#1206 = EDGE_CURVE ( 'NONE', #717, #13076, #1195, .T. ) ;
#1207 = EDGE_LOOP ( 'NONE', ( #4041, #3316, #12995, #12379, #2271, #520, #2141, #10839 ) ) ;
#1208 = EDGE_CURVE ( 'NONE', #9380, #4994, #11562, .T. ) ;
#1209 = VECTOR ( 'NONE', #1133, 1000.000000000000000 ) ;
#1210 = CARTESIAN_POINT ( 'NONE',  ( 45.00000000000000000, 515.4878487013597805, -486.7230258972047636 ) ) ;
#1211 = FACE_OUTER_BOUND ( 'NONE', #7622, .T. ) ;
#1212 = AXIS2_PLACEMENT_3D ( 'NONE', #778, #9719, #6164 ) ;
#1213 = PLANE ( 'NONE',  #3581 ) ;
#1214 = ORIENTED_EDGE ( 'NONE', *, *, #5476, .T. ) ;
#1215 = CARTESIAN_POINT ( 'NONE',  ( -45.00000000000000000, 493.2350855268086320, -508.1801094700848580 ) ) ;
#1216 = DIRECTION ( 'NONE',  ( -0.000000000000000000, -1.000000000000000000, -0.000000000000000000 ) ) ;
#1217 = EDGE_LOOP ( 'NONE', ( #865, #11206, #10156, #13235 ) ) ;
#1218 = PRODUCT_DEFINITION_FORMATION_WITH_SPECIFIED_SOURCE ( 'ANY', '', #9625, .NOT_KNOWN. ) ;
#1219 = PLANE ( 'NONE',  #16820 ) ;
#1220 = EDGE_LOOP ( 'NONE', ( #12300, #2857, #7476, #5756 ) ) ;
#1221 = EDGE_LOOP ( 'NONE', ( #1972, #9774, #15434, #5511 ) ) ;
#1222 = DIRECTION ( 'NONE',  ( 0.000000000000000000, 0.000000000000000000, -1.000000000000000000 ) ) ;
#1223 = EDGE_CURVE ( 'NONE', #16701, #16577, #11838, .T. ) ;
#1224 = AXIS2_PLACEMENT_3D ( 'NONE', #279, #10924, #8345 ) ;
#1225 = ORIENTED_EDGE ( 'NONE', *, *, #10248, .T. ) ;
#1226 = EDGE_LOOP ( 'NONE', ( #8728, #12309 ) ) ;
#1227 = EDGE_CURVE ( 'NONE', #2521, #15829, #12875, .T. ) ;
#1228 = EDGE_CURVE ( 'NONE', #11320, #13664, #3899, .T. ) ;
#1229 = ORIENTED_EDGE ( 'NONE', *, *, #16397, .T. ) ;
#1230 = ADVANCED_FACE ( 'NONE', ( #13135 ), #10307, .F. ) ;
#1231 = CARTESIAN_POINT ( 'NONE',  ( 26.00000000000000355, 19.00000000000000000, -31.00000000000004263 ) ) ;
#1232 = CYLINDRICAL_SURFACE ( 'NONE', #4228, 59.99999999999994316 ) ;
#1233 = VERTEX_POINT ( 'NONE', #11671 ) ;
#1234 = VECTOR ( 'NONE', #7686, 1000.000000000000000 ) ;
#1235 = LINE ( 'NONE', #14372, #6109 ) ;
#1236 = AXIS2_PLACEMENT_3D ( 'NONE', #592, #16216, #5908 ) ;
#1237 = DIRECTION ( 'NONE',  ( 1.000000000000000000, 0.000000000000000000, 0.000000000000000000 ) ) ;
#1238 = ORIENTED_EDGE ( 'NONE', *, *, #14526, .F. ) ;
#1239 = FACE_OUTER_BOUND ( 'NONE', #11636, .T. ) ;
#1240 = LINE ( 'NONE', #2612, #7194 ) ;
#1241 = EDGE_LOOP ( 'NONE', ( #12752, #12919, #4251, #4555 ) ) ;
#1242 = LINE ( 'NONE', #5255, #7128 ) ;
#1243 = ORIENTED_EDGE ( 'NONE', *, *, #286, .T. ) ;
#1244 = DIRECTION ( 'NONE',  ( 1.000000000000000000, -0.000000000000000000, -0.000000000000000000 ) ) ;
#1245 = AXIS2_PLACEMENT_3D ( 'NONE', #2717, #2979, #14407 ) ;
#1246 = ORIENTED_EDGE ( 'NONE', *, *, #9827, .F. ) ;
#1247 = ORIENTED_EDGE ( 'NONE', *, *, #8989, .T. ) ;
#1248 = PLANE ( 'NONE',  #9114 ) ;
#1249 = CARTESIAN_POINT ( 'NONE',  ( -31.00000000000005684, 0.000000000000000000, -23.00000000000000000 ) ) ;
#1250 = CARTESIAN_POINT ( 'NONE',  ( 394.0000000000001137, 339.3157724647196005, -104.9456657433597968 ) ) ;
#1251 = ORIENTED_EDGE ( 'NONE', *, *, #13170, .T. ) ;
#1252 = DIRECTION ( 'NONE',  ( -0.000000000000000000, -0.000000000000000000, 1.000000000000000000 ) ) ;
#1253 = CARTESIAN_POINT ( 'NONE',  ( 0.000000000000000000, 0.000000000000000000, -5.268482129199949959 ) ) ;
#1254 = VECTOR ( 'NONE', #4572, 1000.000000000000000 ) ;
#1255 = DIRECTION ( 'NONE',  ( -1.631319816340925300E-17, -0.000000000000000000, 1.000000000000000000 ) ) ;
#1256 = VECTOR ( 'NONE', #9148, 1000.000000000000000 ) ;
#1257 = LINE ( 'NONE', #16960, #8695 ) ;
#1258 = DIRECTION ( 'NONE',  ( -0.000000000000000000, -1.000000000000000000, 0.000000000000000000 ) ) ;
#1259 = FACE_BOUND ( 'NONE', #12186, .T. ) ;
#1260 = CARTESIAN_POINT ( 'NONE',  ( 449.9999999999998295, 135.5000000000000000, 3.000000000000000000 ) ) ;
#1261 = EDGE_CURVE ( 'NONE', #8474, #4810, #9019, .T. ) ;
#1263 = ORIENTED_EDGE ( 'NONE', *, *, #8409, .F. ) ;
#1262 = EDGE_LOOP ( 'NONE', ( #3431, #9130, #16351, #16557, #16838, #8786, #9972, #3959, #8524 ) ) ;
#1264 = CARTESIAN_POINT ( 'NONE',  ( 40.00000000000000000, 68.00000000000000000, 26.00000000000000355 ) ) ;
#1265 = VECTOR ( 'NONE', #8841, 1000.000000000000227 ) ;
#1266 = EDGE_CURVE ( 'NONE', #6745, #14546, #5394, .T. ) ;
#1267 = CARTESIAN_POINT ( 'NONE',  ( -31.00000000000006395, 19.00000000000000000, 20.99999999999998934 ) ) ;
#1268 = AXIS2_PLACEMENT_3D ( 'NONE', #10126, #1099, #2388 ) ;
#1269 = DIRECTION ( 'NONE',  ( -0.000000000000000000, 1.000000000000000000, -0.000000000000000000 ) ) ;
#1270 = CARTESIAN_POINT ( 'NONE',  ( 25.99999999999998224, 6.000000000000000000, -31.99999999999998579 ) ) ;
#1271 = ORIENTED_EDGE ( 'NONE', *, *, #7467, .F. ) ;
#1272 = DIRECTION ( 'NONE',  ( 0.000000000000000000, 0.000000000000000000, -1.000000000000000000 ) ) ;
#1273 = LINE ( 'NONE', #10299, #16887 ) ;
#1274 = ORIENTED_EDGE ( 'NONE', *, *, #12030, .T. ) ;
#1275 = CARTESIAN_POINT ( 'NONE',  ( -5.000000000000000888, 0.000000000000000000, 22.46376988133006236 ) ) ;
#1276 = LINE ( 'NONE', #14662, #2418 ) ;
#1277 = DIRECTION ( 'NONE',  ( 1.000000000000000000, 0.000000000000000000, 0.000000000000000000 ) ) ;
#1278 = ORIENTED_EDGE ( 'NONE', *, *, #9293, .T. ) ;
#1279 = CIRCLE ( 'NONE', #12264, 10.00000000000061995 ) ;
#1280 = CIRCLE ( 'NONE', #2647, 4.695405383896011919 ) ;
#1281 = CARTESIAN_POINT ( 'NONE',  ( 34.99999999999997868, 8.000000000000000000, 40.00000000000000711 ) ) ;
#1282 = DIRECTION ( 'NONE',  ( 1.000000000000000000, 0.000000000000000000, -0.000000000000000000 ) ) ;
#1283 = ORIENTED_EDGE ( 'NONE', *, *, #7902, .F. ) ;
#1284 = ADVANCED_FACE ( 'NONE', ( #14336 ), #15957, .T. ) ;
#1285 = DIRECTION ( 'NONE',  ( -0.000000000000000000, -1.000000000000000000, -0.000000000000000000 ) ) ;
#1286 = DIRECTION ( 'NONE',  ( 0.000000000000000000, 0.000000000000000000, -1.000000000000000000 ) ) ;
#1287 = CIRCLE ( 'NONE', #14740, 10.00000000000000178 ) ;
#1288 = EDGE_LOOP ( 'NONE', ( #9754, #15029, #5415, #13991 ) ) ;
#1289 = VECTOR ( 'NONE', #11261, 1000.000000000000000 ) ;
#1290 = LINE ( 'NONE', #3707, #3363 ) ;
#1291 = LINE ( 'NONE', #10728, #11364 ) ;
#1292 = EDGE_CURVE ( 'NONE', #13450, #1044, #16815, .T. ) ;
#1293 = LINE ( 'NONE', #11850, #3847 ) ;
#1294 = VERTEX_POINT ( 'NONE', #6413 ) ;
#1295 = FACE_OUTER_BOUND ( 'NONE', #5747, .T. ) ;
#1296 = LINE ( 'NONE', #5147, #15553 ) ;
#1297 = ORIENTED_EDGE ( 'NONE', *, *, #13299, .T. ) ;
#1298 = FACE_OUTER_BOUND ( 'NONE', #8169, .T. ) ;
#1299 = VERTEX_POINT ( 'NONE', #256 ) ;
#1300 = ORIENTED_EDGE ( 'NONE', *, *, #809, .F. ) ;
#1301 = EDGE_CURVE ( 'NONE', #4071, #13919, #1705, .T. ) ;
#1302 = DIRECTION ( 'NONE',  ( 1.000000000000000000, 0.000000000000000000, 0.000000000000000000 ) ) ;
#1303 = ORIENTED_EDGE ( 'NONE', *, *, #13173, .F. ) ;
#1304 = CARTESIAN_POINT ( 'NONE',  ( 0.000000000000000000, 0.000000000000000000, 0.000000000000000000 ) ) ;
#1305 = EDGE_LOOP ( 'NONE', ( #13296, #8825, #115, #607 ) ) ;
#1306 = ORIENTED_EDGE ( 'NONE', *, *, #10791, .T. ) ;
#1307 = LINE ( 'NONE', #26, #15133 ) ;
#1308 = CARTESIAN_POINT ( 'NONE',  ( 39.75350601975127063, 301.2117639810886089, 0.000000000000000000 ) ) ;
#1309 = VECTOR ( 'NONE', #7352, 1000.000000000000000 ) ;
#1310 = ADVANCED_FACE ( 'NONE', ( #13318 ), #9534, .T. ) ;
#1311 = VERTEX_POINT ( 'NONE', #12018 ) ;
#1312 = DIRECTION ( 'NONE',  ( -1.000000000000000000, -0.000000000000000000, -0.000000000000000000 ) ) ;
#1313 = AXIS2_PLACEMENT_3D ( 'NONE', #3228, #8285, #13540 ) ;
#1314 = ADVANCED_FACE ( 'NONE', ( #14592 ), #16137, .T. ) ;
#1315 = DIRECTION ( 'NONE',  ( 1.000000000000000000, 0.000000000000000000, 0.000000000000000000 ) ) ;
#1316 = CARTESIAN_POINT ( 'NONE',  ( 44.99999999999998579, 515.4878487013597805, -521.7230258972047068 ) ) ;
#1317 = EDGE_CURVE ( 'NONE', #8414, #2249, #4170, .T. ) ;
#1318 = ORIENTED_EDGE ( 'NONE', *, *, #16935, .F. ) ;
#1319 = DIRECTION ( 'NONE',  ( 1.000000000000000000, 0.000000000000000000, -0.000000000000000000 ) ) ;
#1320 = DIRECTION ( 'NONE',  ( 0.000000000000000000, 1.000000000000000000, 0.000000000000000000 ) ) ;
#1321 = ORIENTED_EDGE ( 'NONE', *, *, #14943, .T. ) ;
#1322 = EDGE_CURVE ( 'NONE', #15297, #13085, #2233, .T. ) ;
#1323 = EDGE_CURVE ( 'NONE', #14799, #14337, #8320, .T. ) ;
#1324 = EDGE_CURVE ( 'NONE', #2054, #11526, #1422, .T. ) ;
#1325 = FACE_OUTER_BOUND ( 'NONE', #3982, .T. ) ;
#1326 = VERTEX_POINT ( 'NONE', #10906 ) ;
#1327 = DIRECTION ( 'NONE',  ( 0.000000000000000000, 0.000000000000000000, 1.000000000000000000 ) ) ;
#1328 = AXIS2_PLACEMENT_3D ( 'NONE', #1103, #11574, #14250 ) ;
#1329 = SHAPE_REPRESENTATION ( 'Part1', ( #1488 ), #8346 ) ;
#1330 = ORIENTED_EDGE ( 'NONE', *, *, #5308, .T. ) ;
#1331 = ORIENTED_EDGE ( 'NONE', *, *, #8487, .T. ) ;
#1332 = LINE ( 'NONE', #308, #13515 ) ;
#1333 = FACE_OUTER_BOUND ( 'NONE', #14794, .T. ) ;
#1334 = CYLINDRICAL_SURFACE ( 'NONE', #4212, 2.999999999999995559 ) ;
#1335 = ORIENTED_EDGE ( 'NONE', *, *, #8749, .F. ) ;
#1336 = DIRECTION ( 'NONE',  ( 0.000000000000000000, 0.000000000000000000, 1.000000000000000000 ) ) ;
#1337 = CARTESIAN_POINT ( 'NONE',  ( 0.000000000000000000, 234.3157724647196289, -17.15546574335979813 ) ) ;
#1338 = FACE_OUTER_BOUND ( 'NONE', #8908, .T. ) ;
#1339 = VECTOR ( 'NONE', #16363, 1000.000000000000000 ) ;
#1340 = FACE_BOUND ( 'NONE', #1383, .T. ) ;
#1341 = CARTESIAN_POINT ( 'NONE',  ( 37.00000000000003553, -20.00000000000000000, 23.00000000000000355 ) ) ;
#1342 = EDGE_CURVE ( 'NONE', #7123, #3171, #5567, .T. ) ;
#1343 = CARTESIAN_POINT ( 'NONE',  ( -13.11912225705329327, 0.000000000000000000, 0.000000000000000000 ) ) ;
#1344 = DIRECTION ( 'NONE',  ( 0.000000000000000000, 0.000000000000000000, -1.000000000000000000 ) ) ;
#1346 = ORIENTED_EDGE ( 'NONE', *, *, #11561, .T. ) ;
#1345 = ORIENTED_EDGE ( 'NONE', *, *, #16480, .T. ) ;
#1347 = CARTESIAN_POINT ( 'NONE',  ( 17.00000000000000355, 277.8092731128509740, -44.71049682360899169 ) ) ;
#1348 = CIRCLE ( 'NONE', #9342, 17.85000000000000142 ) ;
#1349 = DIRECTION ( 'NONE',  ( -0.000000000000000000, -0.000000000000000000, 1.000000000000000000 ) ) ;
#1350 = CARTESIAN_POINT ( 'NONE',  ( 4.286263797015737285E-15, -3.000000000000000000, -35.00000000000000711 ) ) ;
#1351 = CARTESIAN_POINT ( 'NONE',  ( -9.000000000000001776, 0.000000000000000000, 0.000000000000000000 ) ) ;
#1352 = ORIENTED_EDGE ( 'NONE', *, *, #8341, .F. ) ;
#1353 = LINE ( 'NONE', #6922, #15709 ) ;
#1354 = ADVANCED_FACE ( 'NONE', ( #3083, #8061 ), #15955, .F. ) ;
#1355 = AXIS2_PLACEMENT_3D ( 'NONE', #12281, #16142, #12107 ) ;
#1356 = CARTESIAN_POINT ( 'NONE',  ( 0.000000000000000000, 65.20000000000000284, -5.741599279633704455E-16 ) ) ;
#1357 = ORIENTED_EDGE ( 'NONE', *, *, #12212, .T. ) ;
#1358 = DIRECTION ( 'NONE',  ( 0.000000000000000000, 0.000000000000000000, -1.000000000000000000 ) ) ;
#1359 = DIRECTION ( 'NONE',  ( 1.000000000000000000, -0.000000000000000000, -0.000000000000000000 ) ) ;
#1360 = DIRECTION ( 'NONE',  ( 0.000000000000000000, 0.000000000000000000, -1.000000000000000000 ) ) ;
#1361 = PRODUCT_DEFINITION_SHAPE ( 'NONE', 'NONE',  #16965 ) ;
#1362 = DIRECTION ( 'NONE',  ( -1.000000000000000000, 0.000000000000000000, 0.000000000000000000 ) ) ;
#1363 = DIRECTION ( 'NONE',  ( 0.000000000000000000, 0.6366988521258363232, -0.7711125544961918710 ) ) ;
#1364 = DIRECTION ( 'NONE',  ( 1.000000000000000000, -0.000000000000000000, 0.000000000000000000 ) ) ;
#1365 = VERTEX_POINT ( 'NONE', #1623 ) ;
#1366 = PLANE ( 'NONE',  #691 ) ;
#1367 = VECTOR ( 'NONE', #2102, 1000.000000000000000 ) ;
#1368 = CARTESIAN_POINT ( 'NONE',  ( 30.90550859392621064, 22.88608451763352036, 66.87703344121217697 ) ) ;
#1369 = CIRCLE ( 'NONE', #15902, 13.69540538389598083 ) ;
#1370 = CARTESIAN_POINT ( 'NONE',  ( 20.99999999999996092, 0.000000000000000000, 35.00000000000000711 ) ) ;
#1371 = ORIENTED_EDGE ( 'NONE', *, *, #16022, .T. ) ;
#1372 = DIRECTION ( 'NONE',  ( 0.000000000000000000, 0.9848077530122062440, 0.1736481776669404620 ) ) ;
#1373 = CYLINDRICAL_SURFACE ( 'NONE', #5059, 9.999999999999998224 ) ;
#1374 = CARTESIAN_POINT ( 'NONE',  ( 44.68009836720081296, 275.4439001176564830, -75.00000000000000000 ) ) ;
#1375 = VERTEX_POINT ( 'NONE', #6843 ) ;
#1376 = DIRECTION ( 'NONE',  ( 1.000000000000000000, 0.000000000000000000, -1.156482317317883755E-15 ) ) ;
#1377 = CARTESIAN_POINT ( 'NONE',  ( 31.99999999999998579, 10.00000000000000000, 21.99999999999999645 ) ) ;
#1378 = DIRECTION ( 'NONE',  ( 0.000000000000000000, 0.000000000000000000, -1.000000000000000000 ) ) ;
#1379 = VERTEX_POINT ( 'NONE', #12101 ) ;
#1380 = VECTOR ( 'NONE', #8042, 1000.000000000000000 ) ;
#1381 = AXIS2_PLACEMENT_3D ( 'NONE', #7328, #8638, #13704 ) ;
#1382 = ORIENTED_EDGE ( 'NONE', *, *, #11302, .F. ) ;
#1383 = EDGE_LOOP ( 'NONE', ( #947, #1303 ) ) ;
#1384 = DIRECTION ( 'NONE',  ( 1.000000000000000000, 0.000000000000000000, 0.000000000000000000 ) ) ;
#1385 = ORIENTED_EDGE ( 'NONE', *, *, #5385, .F. ) ;
#1386 = VERTEX_POINT ( 'NONE', #339 ) ;
#1387 =( LENGTH_UNIT ( ) NAMED_UNIT ( * ) SI_UNIT ( .MILLI., .METRE. ) );
#1388 = ADVANCED_FACE ( 'NONE', ( #10815 ), #13110, .T. ) ;
#1389 = VERTEX_POINT ( 'NONE', #11644 ) ;
#1390 = CIRCLE ( 'NONE', #12633, 3.300000000000025135 ) ;
#1391 = VERTEX_POINT ( 'NONE', #15667 ) ;
#1392 = DIRECTION ( 'NONE',  ( -1.000000000000000000, 0.000000000000000000, -0.000000000000000000 ) ) ;
#1393 = DIRECTION ( 'NONE',  ( 0.000000000000000000, 0.000000000000000000, -1.000000000000000000 ) ) ;
#1394 =( REPRESENTATION_RELATIONSHIP ('NONE','NONE', #15822, #8805 ) REPRESENTATION_RELATIONSHIP_WITH_TRANSFORMATION ( #8477 )SHAPE_REPRESENTATION_RELATIONSHIP( ) );
#1395 = EDGE_CURVE ( 'NONE', #5700, #15832, #15760, .T. ) ;
#1396 = ORIENTED_EDGE ( 'NONE', *, *, #9384, .F. ) ;
#1397 = DIRECTION ( 'NONE',  ( 7.900838015626929923E-17, 8.586860021784410058E-33, -1.000000000000000000 ) ) ;
#1398 = DIRECTION ( 'NONE',  ( 0.000000000000000000, 1.000000000000000000, 0.000000000000000000 ) ) ;
#1399 = ORIENTED_EDGE ( 'NONE', *, *, #15739, .F. ) ;
#1400 = CARTESIAN_POINT ( 'NONE',  ( -20.00000000000003197, 0.000000000000000000, 40.00000000000000711 ) ) ;
#1401 = EDGE_LOOP ( 'NONE', ( #12221, #4419, #11440, #8754 ) ) ;
#1402 = LINE ( 'NONE', #298, #15818 ) ;
#1403 = PLANE ( 'NONE',  #13541 ) ;
#1404 = ORIENTED_EDGE ( 'NONE', *, *, #8025, .T. ) ;
#1405 = CIRCLE ( 'NONE', #5517, 30.00000000000002842 ) ;
#1406 = PLANE ( 'NONE',  #6572 ) ;
#1407 = EDGE_LOOP ( 'NONE', ( #8814, #8708, #16892, #8161 ) ) ;
#1408 = DIRECTION ( 'NONE',  ( 0.000000000000000000, 1.000000000000000000, -0.000000000000000000 ) ) ;
#1409 = ADVANCED_FACE ( 'NONE', ( #50 ), #4007, .T. ) ;
#1410 = VERTEX_POINT ( 'NONE', #9065 ) ;
#1411 = VERTEX_POINT ( 'NONE', #13191 ) ;
#1412 =( LENGTH_UNIT ( ) NAMED_UNIT ( * ) SI_UNIT ( .MILLI., .METRE. ) );
#1413 = LINE ( 'NONE', #6379, #1689 ) ;
#1414 = ADVANCED_FACE ( 'NONE', ( #12926 ), #14656, .F. ) ;
#1415 = DIRECTION ( 'NONE',  ( 0.000000000000000000, 0.000000000000000000, 1.000000000000000000 ) ) ;
#1416 = VECTOR ( 'NONE', #9299, 1000.000000000000000 ) ;
#1418 = VERTEX_POINT ( 'NONE', #6382 ) ;
#1417 = EDGE_CURVE ( 'NONE', #12484, #1150, #2881, .T. ) ;
#1420 = EDGE_CURVE ( 'NONE', #785, #15912, #1419, .T. ) ;
#1419 = LINE ( 'NONE', #8024, #5535 ) ;
#1421 = CARTESIAN_POINT ( 'NONE',  ( -55.99999999999989342, 549.5810598491746077, -518.1154249974242703 ) ) ;
#1422 = CIRCLE ( 'NONE', #15411, 35.00000000000000711 ) ;
#1423 = CARTESIAN_POINT ( 'NONE',  ( 1.209468180989048008E-15, 2.719172340231729715E-32, 12.50000000000000000 ) ) ;
#1424 = CIRCLE ( 'NONE', #3885, 3.000000000000002665 ) ;
#1425 = VECTOR ( 'NONE', #2460, 1000.000000000000000 ) ;
#1426 = PLANE ( 'NONE',  #10886 ) ;
#1427 = DIRECTION ( 'NONE',  ( 1.000000000000000000, 0.000000000000000000, 0.000000000000000000 ) ) ;
#1428 = FACE_OUTER_BOUND ( 'NONE', #5494, .T. ) ;
#1430 = ORIENTED_EDGE ( 'NONE', *, *, #150, .F. ) ;
#1429 = VERTEX_POINT ( 'NONE', #14564 ) ;
#1431 = AXIS2_PLACEMENT_3D ( 'NONE', #2052, #8588, #12449 ) ;
#1432 = CARTESIAN_POINT ( 'NONE',  ( 55.99999999999989342, 523.2161522479888163, -502.8936384967199729 ) ) ;
#1433 = CARTESIAN_POINT ( 'NONE',  ( -3.302699999998713665, 285.4366476906446337, 37.52989836422034386 ) ) ;
#1434 = VECTOR ( 'NONE', #7857, 1000.000000000000000 ) ;
#1435 = AXIS2_PLACEMENT_3D ( 'NONE', #7710, #7888, #7399 ) ;
#1436 = CARTESIAN_POINT ( 'NONE',  ( -36.00000000000000711, 6.000000000000000000, -18.00000000000000355 ) ) ;
#1437 = EDGE_CURVE ( 'NONE', #6153, #3748, #10694, .T. ) ;
#1438 = DIRECTION ( 'NONE',  ( 0.000000000000000000, 0.000000000000000000, -1.000000000000000000 ) ) ;
#1439 = EDGE_CURVE ( 'NONE', #6319, #15231, #6639, .T. ) ;
#1440 = ORIENTED_EDGE ( 'NONE', *, *, #5741, .T. ) ;
#1441 = EDGE_CURVE ( 'NONE', #10521, #4694, #2531, .T. ) ;
#1442 = DIRECTION ( 'NONE',  ( -0.000000000000000000, -0.000000000000000000, 1.000000000000000000 ) ) ;
#1443 = CIRCLE ( 'NONE', #3374, 4.695405383896011919 ) ;
#1444 = FACE_OUTER_BOUND ( 'NONE', #15279, .T. ) ;
#1445 = ORIENTED_EDGE ( 'NONE', *, *, #14104, .T. ) ;
#1446 = DIRECTION ( 'NONE',  ( -0.000000000000000000, 1.000000000000000000, -0.000000000000000000 ) ) ;
#1447 = LINE ( 'NONE', #7018, #6190 ) ;
#1448 = DIRECTION ( 'NONE',  ( -1.000000000000000000, -0.000000000000000000, -0.000000000000000000 ) ) ;
#1449 = AXIS2_PLACEMENT_3D ( 'NONE', #3060, #14488, #9418 ) ;
#1450 = LINE ( 'NONE', #11932, #6656 ) ;
#1451 = AXIS2_PLACEMENT_3D ( 'NONE', #6157, #9956, #9795 ) ;
#1452 =( LENGTH_UNIT ( ) NAMED_UNIT ( * ) SI_UNIT ( .MILLI., .METRE. ) );
#1453 = DIRECTION ( 'NONE',  ( 0.000000000000000000, 0.000000000000000000, -1.000000000000000000 ) ) ;
#1454 = EDGE_LOOP ( 'NONE', ( #112, #4903, #15639, #15666 ) ) ;
#1455 = FACE_OUTER_BOUND ( 'NONE', #11040, .T. ) ;
#1456 = AXIS2_PLACEMENT_3D ( 'NONE', #8720, #3559, #8307 ) ;
#1457 = DIRECTION ( 'NONE',  ( 1.000000000000000000, 0.000000000000000000, 0.000000000000000000 ) ) ;
#1458 = CARTESIAN_POINT ( 'NONE',  ( -270.0000000000000000, 512.1906115401388888, -11.00000000000000000 ) ) ;
#1459 = VERTEX_POINT ( 'NONE', #1163 ) ;
#1460 = AXIS2_PLACEMENT_3D ( 'NONE', #15518, #13026, #11469 ) ;
#1461 = AXIS2_PLACEMENT_3D ( 'NONE', #8764, #11423, #14176 ) ;
#1462 = AXIS2_PLACEMENT_3D ( 'NONE', #6295, #6467, #15664 ) ;
#1463 = DIRECTION ( 'NONE',  ( 0.000000000000000000, -1.000000000000000000, 0.000000000000000000 ) ) ;
#1464 = CARTESIAN_POINT ( 'NONE',  ( -55.99999999999989342, 473.6663340069157471, -536.1966447803968094 ) ) ;
#1465 = FACE_OUTER_BOUND ( 'NONE', #7870, .T. ) ;
#1466 = EDGE_LOOP ( 'NONE', ( #7727, #15131, #2330, #10352, #8900, #4321 ) ) ;
#1467 = PLANE ( 'NONE',  #4490 ) ;
#1468 = CYLINDRICAL_SURFACE ( 'NONE', #10100, 7.500000000000003553 ) ;
#1469 = CARTESIAN_POINT ( 'NONE',  ( 20.99999999999996092, -20.00000000000000000, 35.00000000000000711 ) ) ;
#1470 = ORIENTED_EDGE ( 'NONE', *, *, #15068, .F. ) ;
#1471 = CIRCLE ( 'NONE', #6667, 12.64814671169700055 ) ;
#1472 = CARTESIAN_POINT ( 'NONE',  ( -440.0000000000000568, 425.7506394335853201, -11.00000000000000000 ) ) ;
#1473 = EDGE_LOOP ( 'NONE', ( #2266, #6265, #690, #7755, #616, #13974 ) ) ;
#1474 = ORIENTED_EDGE ( 'NONE', *, *, #16537, .T. ) ;
#1475 = CARTESIAN_POINT ( 'NONE',  ( 55.99999999999989342, 473.6663340069158039, -575.6402177818052905 ) ) ;
#1476 = CIRCLE ( 'NONE', #6943, 187.4999999999998863 ) ;
#1477 = VECTOR ( 'NONE', #8385, 1000.000000000000000 ) ;
#1478 = ORIENTED_EDGE ( 'NONE', *, *, #5200, .T. ) ;
#1479 = DIRECTION ( 'NONE',  ( 1.000000000000000000, 0.000000000000000000, 0.000000000000000000 ) ) ;
#1480 = AXIS2_PLACEMENT_3D ( 'NONE', #235, #6477, #4179 ) ;
#1481 = VERTEX_POINT ( 'NONE', #11992 ) ;
#1482 = AXIS2_PLACEMENT_3D ( 'NONE', #1275, #11751, #14075 ) ;
#1483 = EDGE_CURVE ( 'NONE', #15480, #13498, #15846, .T. ) ;
#1484 = EDGE_LOOP ( 'NONE', ( #575, #11394 ) ) ;
#1485 = DIRECTION ( 'NONE',  ( 0.000000000000000000, 0.000000000000000000, 1.000000000000000000 ) ) ;
#1486 = DIRECTION ( 'NONE',  ( 0.9998870921963913805, 0.01502673813723916230, 0.000000000000000000 ) ) ;
#1487 = VECTOR ( 'NONE', #16481, 1000.000000000000000 ) ;
#1488 = AXIS2_PLACEMENT_3D ( 'NONE', #3280, #8693, #15217 ) ;
#1489 = ORIENTED_EDGE ( 'NONE', *, *, #11917, .F. ) ;
#1490 = DIRECTION ( 'NONE',  ( -0.000000000000000000, -0.000000000000000000, -1.000000000000000000 ) ) ;
#1491 = AXIS2_PLACEMENT_3D ( 'NONE', #16666, #5064, #16910 ) ;
#1492 = PLANE ( 'NONE',  #8426 ) ;
#1493 = ORIENTED_EDGE ( 'NONE', *, *, #3119, .T. ) ;
#1494 = VECTOR ( 'NONE', #2847, 1000.000000000000000 ) ;
#1495 = FACE_OUTER_BOUND ( 'NONE', #10710, .T. ) ;
#1496 = VERTEX_POINT ( 'NONE', #10362 ) ;
#1497 = CARTESIAN_POINT ( 'NONE',  ( -37.00000000000000711, 0.000000000000000000, 23.00000000000000000 ) ) ;
#1498 = CARTESIAN_POINT ( 'NONE',  ( 0.000000000000000000, 0.000000000000000000, 0.000000000000000000 ) ) ;
#1499 = ORIENTED_EDGE ( 'NONE', *, *, #3451, .F. ) ;
#1500 = DIRECTION ( 'NONE',  ( 0.000000000000000000, 0.000000000000000000, 1.000000000000000000 ) ) ;
#1501 = VERTEX_POINT ( 'NONE', #13024 ) ;
#1502 = EDGE_CURVE ( 'NONE', #12140, #1004, #15137, .T. ) ;
#1503 = CARTESIAN_POINT ( 'NONE',  ( -20.00000000000003197, 3.000000000000000000, 40.00000000000000711 ) ) ;
#1504 = PRODUCT_DEFINITION_FORMATION_WITH_SPECIFIED_SOURCE ( 'ANY', '', #2165, .NOT_KNOWN. ) ;
#1505 = AXIS2_PLACEMENT_3D ( 'NONE', #1421, #7596, #8993 ) ;
#1506 = VERTEX_POINT ( 'NONE', #14484 ) ;
#1507 = ORIENTED_EDGE ( 'NONE', *, *, #10893, .T. ) ;
#1508 = PLANE ( 'NONE',  #10751 ) ;
#1509 = DIRECTION ( 'NONE',  ( 0.000000000000000000, -7.137148015447440312E-15, 1.000000000000000000 ) ) ;
#1510 = CARTESIAN_POINT ( 'NONE',  ( 10.00000000000000000, 374.2147300931088694, -220.2054496871573974 ) ) ;
#1511 = VERTEX_POINT ( 'NONE', #10436 ) ;
#1512 = DIRECTION ( 'NONE',  ( -1.000000000000000000, -0.000000000000000000, -0.000000000000000000 ) ) ;
#1513 = PRODUCT ( 'Part1', 'Part1', '', ( #12628 ) ) ;
#1514 = CARTESIAN_POINT ( 'NONE',  ( 31.00000000000002842, 68.00000000000000000, 23.00000000000001066 ) ) ;
#1515 = EDGE_CURVE ( 'NONE', #12302, #1865, #3914, .T. ) ;
#1516 = DIRECTION ( 'NONE',  ( 0.000000000000000000, 0.000000000000000000, -1.000000000000000000 ) ) ;
#1517 = DIRECTION ( 'NONE',  ( -1.000000000000000000, -0.000000000000000000, -0.000000000000000000 ) ) ;
#1518 = DIRECTION ( 'NONE',  ( 0.000000000000000000, 0.000000000000000000, 1.000000000000000000 ) ) ;
#1519 = VECTOR ( 'NONE', #4527, 1000.000000000000114 ) ;
#1520 = DIRECTION ( 'NONE',  ( 0.000000000000000000, 0.000000000000000000, -1.000000000000000000 ) ) ;
#1522 = ORIENTED_EDGE ( 'NONE', *, *, #10341, .T. ) ;
#1521 = EDGE_LOOP ( 'NONE', ( #2199, #6012 ) ) ;
#1523 = EDGE_CURVE ( 'NONE', #16479, #11116, #10748, .T. ) ;
#1524 = EDGE_CURVE ( 'NONE', #12261, #1137, #6552, .T. ) ;
#1525 = DIRECTION ( 'NONE',  ( 0.000000000000000000, 0.000000000000000000, -1.000000000000000000 ) ) ;
#1526 = EDGE_CURVE ( 'NONE', #9900, #3550, #2708, .T. ) ;
#1527 = LINE ( 'NONE', #12178, #613 ) ;
#1528 = DIRECTION ( 'NONE',  ( 0.000000000000000000, 0.000000000000000000, 1.000000000000000000 ) ) ;
#1529 = CARTESIAN_POINT ( 'NONE',  ( 394.0000000000001137, 234.3157724647196289, -110.6822657433598067 ) ) ;
#1530 = ORIENTED_EDGE ( 'NONE', *, *, #2037, .F. ) ;
#1531 = AXIS2_PLACEMENT_3D ( 'NONE', #5439, #8110, #13182 ) ;
#1532 = CARTESIAN_POINT ( 'NONE',  ( 25.99999999999997513, 0.000000000000000000, 31.00000000000003553 ) ) ;
#1533 = CARTESIAN_POINT ( 'NONE',  ( -26.00000000000002842, 0.000000000000000000, -39.99999999999999289 ) ) ;
#1535 = ADVANCED_FACE ( 'NONE', ( #9325 ), #2789, .F. ) ;
#1534 = ORIENTED_EDGE ( 'NONE', *, *, #6080, .F. ) ;
#1536 = DIRECTION ( 'NONE',  ( 0.000000000000000000, 0.000000000000000000, 1.000000000000000000 ) ) ;
#1537 = LINE ( 'NONE', #14506, #12511 ) ;
#1538 = DIRECTION ( 'NONE',  ( 1.000000000000000000, 0.000000000000000000, 0.000000000000000000 ) ) ;
#1539 = DIRECTION ( 'NONE',  ( 0.000000000000000000, 1.000000000000000000, 0.000000000000000000 ) ) ;
#1540 = CARTESIAN_POINT ( 'NONE',  ( -46.99999999999988631, 493.2350855268086320, -508.1801094700848580 ) ) ;
#1541 = CARTESIAN_POINT ( 'NONE',  ( 0.000000000000000000, -3.000000000000000000, 0.000000000000000000 ) ) ;
#1542 = VERTEX_POINT ( 'NONE', #8386 ) ;
#1543 = ADVANCED_FACE ( 'NONE', ( #16358 ), #10953, .T. ) ;
#1544 = EDGE_CURVE ( 'NONE', #10621, #1954, #3053, .T. ) ;
#1545 = AXIS2_PLACEMENT_3D ( 'NONE', #6781, #14701, #6859 ) ;
#1546 = EDGE_CURVE ( 'NONE', #16912, #12051, #2967, .T. ) ;
#1547 = PLANE ( 'NONE',  #13313 ) ;
#1548 = VECTOR ( 'NONE', #1697, 1000.000000000000000 ) ;
#1549 = EDGE_CURVE ( 'NONE', #13438, #10961, #4514, .T. ) ;
#1550 = CARTESIAN_POINT ( 'NONE',  ( -26.00000000000000000, 19.00000000000000000, 40.00000000000001421 ) ) ;
#1551 = ORIENTED_EDGE ( 'NONE', *, *, #4342, .T. ) ;
#1552 = DIRECTION ( 'NONE',  ( 0.000000000000000000, -1.000000000000000000, 0.000000000000000000 ) ) ;
#1553 = LINE ( 'NONE', #14601, #2317 ) ;
#1554 = VECTOR ( 'NONE', #4294, 1000.000000000000227 ) ;
#1555 = DIRECTION ( 'NONE',  ( 0.000000000000000000, 0.000000000000000000, 1.000000000000000000 ) ) ;
#1556 = ORIENTED_EDGE ( 'NONE', *, *, #12023, .T. ) ;
#1557 = AXIS2_PLACEMENT_3D ( 'NONE', #2859, #4333, #8184 ) ;
#1558 = DIRECTION ( 'NONE',  ( 1.000000000000000000, -0.000000000000000000, -0.000000000000000000 ) ) ;
#1559 = DIRECTION ( 'NONE',  ( -0.000000000000000000, -1.000000000000000000, -0.000000000000000000 ) ) ;
#1560 = CYLINDRICAL_SURFACE ( 'NONE', #5660, 3.300000000000011369 ) ;
#1561 = VERTEX_POINT ( 'NONE', #9837 ) ;
#1562 = CARTESIAN_POINT ( 'NONE',  ( 55.99999999999989342, 549.5810598491749488, -575.3306267969850296 ) ) ;
#1563 = ORIENTED_EDGE ( 'NONE', *, *, #4283, .T. ) ;
#1564 = ORIENTED_EDGE ( 'NONE', *, *, #10984, .F. ) ;
#1565 = LINE ( 'NONE', #1475, #11918 ) ;
#1566 = EDGE_CURVE ( 'NONE', #11526, #2054, #6796, .T. ) ;
#1567 = VERTEX_POINT ( 'NONE', #11034 ) ;
#1568 =( NAMED_UNIT ( * ) PLANE_ANGLE_UNIT ( ) SI_UNIT ( $, .RADIAN. ) );
#1569 = VECTOR ( 'NONE', #15501, 1000.000000000000000 ) ;
#1570 = CIRCLE ( 'NONE', #11165, 4.000000000000003553 ) ;
#1571 = ORIENTED_EDGE ( 'NONE', *, *, #9411, .T. ) ;
#1572 = VERTEX_POINT ( 'NONE', #8201 ) ;
#1573 = CARTESIAN_POINT ( 'NONE',  ( 35.00000000000000711, 19.00000000000000000, 20.99999999999999289 ) ) ;
#1574 = DIRECTION ( 'NONE',  ( -0.000000000000000000, -0.000000000000000000, 1.000000000000000000 ) ) ;
#1575 = ORIENTED_EDGE ( 'NONE', *, *, #3185, .T. ) ;
#1576 = DIRECTION ( 'NONE',  ( -0.000000000000000000, 1.000000000000000000, -0.000000000000000000 ) ) ;
#1577 = ADVANCED_FACE ( 'NONE', ( #10872 ), #6992, .T. ) ;
#1578 = LINE ( 'NONE', #8267, #7825 ) ;
#1579 = ORIENTED_EDGE ( 'NONE', *, *, #3732, .F. ) ;
#1580 = AXIS2_PLACEMENT_3D ( 'NONE', #12541, #13837, #16575 ) ;
#1581 = DIRECTION ( 'NONE',  ( -0.000000000000000000, -1.000000000000000000, -0.000000000000000000 ) ) ;
#1582 = ORIENTED_EDGE ( 'NONE', *, *, #8753, .T. ) ;
#1583 = FACE_OUTER_BOUND ( 'NONE', #11974, .T. ) ;
#1584 = LINE ( 'NONE', #4248, #7741 ) ;
#1585 = ORIENTED_EDGE ( 'NONE', *, *, #5499, .T. ) ;
#1586 = CARTESIAN_POINT ( 'NONE',  ( 34.00000000000002842, 3.000000000000000000, 26.00000000000000355 ) ) ;
#1587 = ORIENTED_EDGE ( 'NONE', *, *, #12196, .F. ) ;
#1588 =( NAMED_UNIT ( * ) PLANE_ANGLE_UNIT ( ) SI_UNIT ( $, .RADIAN. ) );
#1589 = DIRECTION ( 'NONE',  ( -0.000000000000000000, -0.000000000000000000, 1.000000000000000000 ) ) ;
#1590 = EDGE_LOOP ( 'NONE', ( #4710, #5553, #13840, #8321, #11637 ) ) ;
#1591 = VECTOR ( 'NONE', #12521, 1000.000000000000000 ) ;
#1592 = EDGE_LOOP ( 'NONE', ( #3233, #16653, #12543, #5964 ) ) ;
#1593 = PLANE ( 'NONE',  #623 ) ;
#1594 = DIRECTION ( 'NONE',  ( 0.000000000000000000, 1.000000000000000000, 1.224646799147353207E-16 ) ) ;
#1595 = CARTESIAN_POINT ( 'NONE',  ( -22.99999999999999645, 0.000000000000000000, 37.00000000000002132 ) ) ;
#1596 = DIRECTION ( 'NONE',  ( 0.000000000000000000, -0.3420201433256630508, -0.9396926207859104263 ) ) ;
#1597 = CARTESIAN_POINT ( 'NONE',  ( 394.0000000000001137, 240.7889724647196488, -10.68226574335980139 ) ) ;
#1598 = DIRECTION ( 'NONE',  ( -0.000000000000000000, 1.000000000000000000, -0.000000000000000000 ) ) ;
#1599 = CARTESIAN_POINT ( 'NONE',  ( 449.9999999999998295, 135.5000000000000000, 3.000000000000000000 ) ) ;
#1600 = CARTESIAN_POINT ( 'NONE',  ( 31.81980515339464333, 0.000000000000000000, 28.51980515339463906 ) ) ;
#1601 = CARTESIAN_POINT ( 'NONE',  ( 10.00000000000000000, 34.88079231221936283, 28.80067286797032722 ) ) ;
#1602 = CYLINDRICAL_SURFACE ( 'NONE', #1480, 13.69540538389596485 ) ;
#1603 = AXIS2_PLACEMENT_3D ( 'NONE', #15323, #6274, #8796 ) ;
#1604 = CARTESIAN_POINT ( 'NONE',  ( 19.99999999999995381, 3.000000000000000000, -36.99999999999999289 ) ) ;
#1606 = VERTEX_POINT ( 'NONE', #12247 ) ;
#1605 = VERTEX_POINT ( 'NONE', #9583 ) ;
#1607 = CARTESIAN_POINT ( 'NONE',  ( 26.00000000000000355, 19.00000000000000000, -31.00000000000003908 ) ) ;
#1608 = CARTESIAN_POINT ( 'NONE',  ( 0.000000000000000000, 339.3157724647196005, -10.68226574335978718 ) ) ;
#1609 = ADVANCED_FACE ( 'NONE', ( #644 ), #14742, .T. ) ;
#1610 = LINE ( 'NONE', #4441, #12374 ) ;
#1611 = DIRECTION ( 'NONE',  ( 0.000000000000000000, 0.000000000000000000, 1.000000000000000000 ) ) ;
#1612 = ORIENTED_EDGE ( 'NONE', *, *, #2734, .F. ) ;
#1613 = DIRECTION ( 'NONE',  ( 0.000000000000000000, 0.000000000000000000, -1.000000000000000000 ) ) ;
#1614 = EDGE_CURVE ( 'NONE', #793, #11643, #14822, .T. ) ;
#1615 = LINE ( 'NONE', #6834, #14730 ) ;
#1616 = ORIENTED_EDGE ( 'NONE', *, *, #245, .T. ) ;
#1617 = CARTESIAN_POINT ( 'NONE',  ( 414.7091847417151484, 350.3558646104334571, -10.00000000000000000 ) ) ;
#1618 = DIRECTION ( 'NONE',  ( 1.000000000000000000, 0.000000000000000000, 0.000000000000000000 ) ) ;
#1619 = FACE_BOUND ( 'NONE', #13605, .T. ) ;
#1620 = ORIENTED_EDGE ( 'NONE', *, *, #15280, .T. ) ;
#1621 = DIRECTION ( 'NONE',  ( 0.000000000000000000, 1.000000000000000000, 1.224646799147353207E-16 ) ) ;
#1622 = CARTESIAN_POINT ( 'NONE',  ( -0.9999999999999991118, 0.000000000000000000, 0.000000000000000000 ) ) ;
#1623 = CARTESIAN_POINT ( 'NONE',  ( 394.0000000000001137, 240.7889724647196488, -110.6822657433598067 ) ) ;
#1624 = ORIENTED_EDGE ( 'NONE', *, *, #4255, .F. ) ;
#1625 = DIRECTION ( 'NONE',  ( -0.000000000000000000, 1.000000000000000000, -0.000000000000000000 ) ) ;
#1626 = DIRECTION ( 'NONE',  ( -1.000000000000000000, -0.000000000000000000, 0.000000000000000000 ) ) ;
#1627 = EDGE_CURVE ( 'NONE', #8729, #9952, #15064, .T. ) ;
#1628 = CIRCLE ( 'NONE', #14257, 84.99999999999997158 ) ;
#1629 = VERTEX_POINT ( 'NONE', #14992 ) ;
#1630 = CARTESIAN_POINT ( 'NONE',  ( 1.250085104875786612E-12, 218.4499468633019603, 287.1312267635915987 ) ) ;
#1631 = EDGE_CURVE ( 'NONE', #16404, #4508, #9674, .T. ) ;
#1632 = DIRECTION ( 'NONE',  ( 0.000000000000000000, 0.000000000000000000, -1.000000000000000000 ) ) ;
#1633 = ADVANCED_FACE ( 'NONE', ( #16017 ), #3151, .F. ) ;
#1634 = EDGE_CURVE ( 'NONE', #13622, #365, #11121, .T. ) ;
#1635 = CARTESIAN_POINT ( 'NONE',  ( 10.00000000000000000, 435.2933666400819561, -550.3792044179907634 ) ) ;
#1636 = EDGE_LOOP ( 'NONE', ( #9639, #14899, #7557, #14166 ) ) ;
#1637 = CARTESIAN_POINT ( 'NONE',  ( -2.736197741142289506E-16, 217.7170024689957586, 287.2045212030222388 ) ) ;
#1638 = ADVANCED_FACE ( 'NONE', ( #12325 ), #13674, .T. ) ;
#1639 = CARTESIAN_POINT ( 'NONE',  ( 10.00000000000000000, 309.2289037985885898, -83.18019484660915452 ) ) ;
#1640 = CARTESIAN_POINT ( 'NONE',  ( -23.00000000000002487, 0.000000000000000000, -36.99999999999999289 ) ) ;
#1641 = VERTEX_POINT ( 'NONE', #13702 ) ;
#1642 = FILL_AREA_STYLE_COLOUR ( '', #5591 ) ;
#1643 = ORIENTED_EDGE ( 'NONE', *, *, #7318, .F. ) ;
#1644 = VERTEX_POINT ( 'NONE', #312 ) ;
#1645 = VECTOR ( 'NONE', #16850, 1000.000000000000000 ) ;
#1646 = DIRECTION ( 'NONE',  ( -3.854941057726247958E-16, 0.000000000000000000, 1.000000000000000000 ) ) ;
#1647 = EDGE_LOOP ( 'NONE', ( #12569, #2644, #3350, #4243 ) ) ;
#1648 = PRODUCT_CONTEXT ( 'NONE', #7958, 'mechanical' ) ;
#1649 = ORIENTED_EDGE ( 'NONE', *, *, #7457, .T. ) ;
#1650 = ORIENTED_EDGE ( 'NONE', *, *, #9582, .T. ) ;
#1651 = FACE_OUTER_BOUND ( 'NONE', #547, .T. ) ;
#1652 = EDGE_CURVE ( 'NONE', #7313, #10036, #5533, .T. ) ;
#1653 = CARTESIAN_POINT ( 'NONE',  ( -54.99999999999999289, 658.4713480608917280, -425.4301204538002139 ) ) ;
#1654 = EDGE_CURVE ( 'NONE', #1299, #4138, #2093, .T. ) ;
#1655 = AXIS2_PLACEMENT_3D ( 'NONE', #15556, #12887, #15805 ) ;
#1656 = ORIENTED_EDGE ( 'NONE', *, *, #1437, .T. ) ;
#1658 = CYLINDRICAL_SURFACE ( 'NONE', #12715, 13.69540538389601991 ) ;
#1657 = CONICAL_SURFACE ( 'NONE', #11250, 13.62500000000000000, 0.2281026282799422378 ) ;
#1659 = EDGE_CURVE ( 'NONE', #9059, #747, #4069, .T. ) ;
#1660 = DIRECTION ( 'NONE',  ( 0.000000000000000000, 0.3746065934159049093, 0.9271838545667903109 ) ) ;
#1661 = ORIENTED_EDGE ( 'NONE', *, *, #1858, .T. ) ;
#1662 = CARTESIAN_POINT ( 'NONE',  ( 0.000000000000000000, 435.2933666400819561, -525.1288175801793159 ) ) ;
#1663 = ORIENTED_EDGE ( 'NONE', *, *, #6779, .T. ) ;
#1664 = CARTESIAN_POINT ( 'NONE',  ( 19.99999999999995381, 3.000000000000000000, -39.99999999999999289 ) ) ;
#1665 = DIRECTION ( 'NONE',  ( -0.000000000000000000, -1.000000000000000000, -0.000000000000000000 ) ) ;
#1666 = ORIENTED_EDGE ( 'NONE', *, *, #14517, .F. ) ;
#1667 = DIRECTION ( 'NONE',  ( 0.000000000000000000, 0.000000000000000000, 1.000000000000000000 ) ) ;
#1668 = EDGE_LOOP ( 'NONE', ( #1824, #8368, #1872, #8991, #277 ) ) ;
#1669 = DIRECTION ( 'NONE',  ( 0.000000000000000000, 1.000000000000000000, 0.000000000000000000 ) ) ;
#1670 = VECTOR ( 'NONE', #12977, 1000.000000000000000 ) ;
#1671 = ORIENTED_EDGE ( 'NONE', *, *, #6132, .T. ) ;
#1672 = ORIENTED_EDGE ( 'NONE', *, *, #4289, .F. ) ;
#1673 = CIRCLE ( 'NONE', #3049, 13.69540538389601991 ) ;
#1674 = CARTESIAN_POINT ( 'NONE',  ( 37.00000000000000000, 68.00000000000000000, 23.00000000000001066 ) ) ;
#1675 = LINE ( 'NONE', #14653, #3677 ) ;
#1676 = DIRECTION ( 'NONE',  ( -0.000000000000000000, -1.000000000000000000, -0.000000000000000000 ) ) ;
#1677 = FACE_OUTER_BOUND ( 'NONE', #1217, .T. ) ;
#1678 = VECTOR ( 'NONE', #10103, 1000.000000000000000 ) ;
#1679 = CARTESIAN_POINT ( 'NONE',  ( 2.799999999999999822, 0.000000000000000000, 0.000000000000000000 ) ) ;
#1680 = CARTESIAN_POINT ( 'NONE',  ( 54.99999999999999289, 173.0499717945046996, 146.7982946275220968 ) ) ;
#1681 = LINE ( 'NONE', #12077, #14454 ) ;
#1682 = LINE ( 'NONE', #14664, #11577 ) ;
#1683 = DIRECTION ( 'NONE',  ( 0.000000000000000000, 0.000000000000000000, -1.000000000000000000 ) ) ;
#1684 = DIRECTION ( 'NONE',  ( 0.000000000000000000, 0.000000000000000000, -1.000000000000000000 ) ) ;
#1686 = EDGE_LOOP ( 'NONE', ( #4706, #4435, #4885, #9982 ) ) ;
#1685 = VERTEX_POINT ( 'NONE', #4658 ) ;
#1687 = DIRECTION ( 'NONE',  ( -3.854941057726250916E-16, 0.000000000000000000, -1.000000000000000000 ) ) ;
#1688 = EDGE_CURVE ( 'NONE', #985, #9484, #6238, .T. ) ;
#1689 = VECTOR ( 'NONE', #12922, 1000.000000000000000 ) ;
#1690 = CARTESIAN_POINT ( 'NONE',  ( -45.00000000000000000, 523.2161522479893847, -604.2478186815853860 ) ) ;
#1691 = CARTESIAN_POINT ( 'NONE',  ( 10.00000000000000000, 372.8685141053783241, -146.8198051533979935 ) ) ;
#1692 = CARTESIAN_POINT ( 'NONE',  ( -39.99999999999997868, -20.00000000000000000, -19.99999999999999645 ) ) ;
#1693 = VERTEX_POINT ( 'NONE', #12655 ) ;
#1694 = AXIS2_PLACEMENT_3D ( 'NONE', #15698, #3945, #9187 ) ;
#1695 = AXIS2_PLACEMENT_3D ( 'NONE', #1075, #3909, #2275 ) ;
#1696 = CARTESIAN_POINT ( 'NONE',  ( 46.99999999999988631, 493.2350855268092573, -598.9613477082210693 ) ) ;
#1697 = DIRECTION ( 'NONE',  ( -0.000000000000000000, -1.000000000000000000, -0.000000000000000000 ) ) ;
#1698 = VERTEX_POINT ( 'NONE', #13953 ) ;
#1699 = CARTESIAN_POINT ( 'NONE',  ( -40.00000000000000000, 68.00000000000000000, -25.99999999999999645 ) ) ;
#1700 = CARTESIAN_POINT ( 'NONE',  ( -21.00000000000002842, 0.000000000000000000, -34.99999999999999289 ) ) ;
#1701 = CARTESIAN_POINT ( 'NONE',  ( 44.68009836720079875, 352.3758082234937206, 0.000000000000000000 ) ) ;
#1702 = VECTOR ( 'NONE', #11528, 1000.000000000000000 ) ;
#1703 = EDGE_CURVE ( 'NONE', #8258, #276, #816, .T. ) ;
#1704 = DIRECTION ( 'NONE',  ( 1.000000000000000000, 0.000000000000000000, 0.000000000000000000 ) ) ;
#1705 = LINE ( 'NONE', #16054, #16773 ) ;
#1706 = ORIENTED_EDGE ( 'NONE', *, *, #1, .T. ) ;
#1707 = VECTOR ( 'NONE', #2650, 1000.000000000000000 ) ;
#1708 = DIRECTION ( 'NONE',  ( 0.000000000000000000, 0.000000000000000000, 1.000000000000000000 ) ) ;
#1709 = PRESENTATION_LAYER_ASSIGNMENT (  '', '', ( #8568 ) ) ;
#1710 = EDGE_CURVE ( 'NONE', #963, #13664, #5708, .T. ) ;
#1711 = DIRECTION ( 'NONE',  ( -0.000000000000000000, -1.000000000000000000, 0.000000000000000000 ) ) ;
#1712 =( NAMED_UNIT ( * ) SI_UNIT ( $, .STERADIAN. ) SOLID_ANGLE_UNIT ( ) );
#1713 = VECTOR ( 'NONE', #16909, 1000.000000000000000 ) ;
#1714 = ORIENTED_EDGE ( 'NONE', *, *, #15609, .T. ) ;
#1715 = LINE ( 'NONE', #13412, #8835 ) ;
#1716 = UNCERTAINTY_MEASURE_WITH_UNIT (LENGTH_MEASURE( 1.000000000000000082E-05 ), #13062, 'distance_accuracy_value', 'NONE');
#1717 = LINE ( 'NONE', #5900, #6701 ) ;
#1718 = DIRECTION ( 'NONE',  ( 0.000000000000000000, 0.000000000000000000, 1.000000000000000000 ) ) ;
#1719 = VERTEX_POINT ( 'NONE', #6033 ) ;
#1720 = PLANE ( 'NONE',  #7764 ) ;
#1721 = VECTOR ( 'NONE', #8206, 1000.000000000000000 ) ;
#1722 = TOROIDAL_SURFACE ( 'NONE', #15152, 4.695405383895982609, 9.000000000000000000 ) ;
#1723 = CYLINDRICAL_SURFACE ( 'NONE', #13950, 25.25038683781155413 ) ;
#1724 = CARTESIAN_POINT ( 'NONE',  ( 26.00000000000000711, 0.000000000000000000, -31.00000000000002487 ) ) ;
#1725 = ORIENTED_EDGE ( 'NONE', *, *, #3322, .F. ) ;
#1726 = EDGE_CURVE ( 'NONE', #7051, #8672, #11201, .T. ) ;
#1727 = DIRECTION ( 'NONE',  ( -1.000000000000000000, 0.000000000000000000, 0.000000000000000000 ) ) ;
#1728 = ADVANCED_FACE ( 'NONE', ( #894 ), #735, .F. ) ;
#1729 = EDGE_LOOP ( 'NONE', ( #2488, #15881, #3895, #9781 ) ) ;
#1730 = ORIENTED_EDGE ( 'NONE', *, *, #9551, .F. ) ;
#1731 = AXIS2_PLACEMENT_3D ( 'NONE', #16127, #4659, #3075 ) ;
#1732 = DIRECTION ( 'NONE',  ( 0.000000000000000000, 0.000000000000000000, 1.000000000000000000 ) ) ;
#1733 = ORIENTED_EDGE ( 'NONE', *, *, #3415, .T. ) ;
#1734 = EDGE_CURVE ( 'NONE', #14532, #4729, #11367, .T. ) ;
#1735 =( NAMED_UNIT ( * ) SI_UNIT ( $, .STERADIAN. ) SOLID_ANGLE_UNIT ( ) );
#1736 = VECTOR ( 'NONE', #14208, 1000.000000000000000 ) ;
#1737 = ADVANCED_FACE ( 'NONE', ( #4999 ), #6117, .F. ) ;
#1738 = ADVANCED_FACE ( 'NONE', ( #16680 ), #4747, .T. ) ;
#1739 = VECTOR ( 'NONE', #2775, 1000.000000000000000 ) ;
#1740 = AXIS2_PLACEMENT_3D ( 'NONE', #4442, #15942, #16125 ) ;
#1741 = ORIENTED_EDGE ( 'NONE', *, *, #13457, .F. ) ;
#1742 = ORIENTED_EDGE ( 'NONE', *, *, #4581, .T. ) ;
#1743 = FACE_BOUND ( 'NONE', #9478, .T. ) ;
#1744 = LINE ( 'NONE', #6010, #6960 ) ;
#1745 = VECTOR ( 'NONE', #16856, 1000.000000000000000 ) ;
#1746 = VERTEX_POINT ( 'NONE', #11276 ) ;
#1747 = CARTESIAN_POINT ( 'NONE',  ( -40.00000000000000000, 68.00000000000000000, 26.00000000000000355 ) ) ;
#1748 = CARTESIAN_POINT ( 'NONE',  ( 31.00000000000001776, 10.00000000000000000, -25.99999999999999645 ) ) ;
#1749 = EDGE_LOOP ( 'NONE', ( #3024, #5307, #10350, #1766 ) ) ;
#1750 =( GEOMETRIC_REPRESENTATION_CONTEXT ( 3 ) GLOBAL_UNCERTAINTY_ASSIGNED_CONTEXT ( ( #6219 ) ) GLOBAL_UNIT_ASSIGNED_CONTEXT ( ( #14018, #549, #9750 ) ) REPRESENTATION_CONTEXT ( 'NONE', 'WORKASPACE' ) );
#1751 = AXIS2_PLACEMENT_3D ( 'NONE', #11035, #5792, #3561 ) ;
#1752 = ADVANCED_FACE ( 'NONE', ( #2255 ), #10166, .T. ) ;
#1753 = DIRECTION ( 'NONE',  ( -1.000000000000000000, -0.000000000000000000, 0.000000000000000000 ) ) ;
#1754 = AXIS2_PLACEMENT_3D ( 'NONE', #12159, #10609, #15844 ) ;
#1755 = VERTEX_POINT ( 'NONE', #10003 ) ;
#1756 = FACE_OUTER_BOUND ( 'NONE', #15388, .T. ) ;
#1757 = DIRECTION ( 'NONE',  ( -0.000000000000000000, -1.000000000000000000, -0.000000000000000000 ) ) ;
#1758 = EDGE_LOOP ( 'NONE', ( #15888, #16873, #10157, #8053, #8499, #10175 ) ) ;
#1759 = VERTEX_POINT ( 'NONE', #7482 ) ;
#1760 = EDGE_CURVE ( 'NONE', #4729, #13306, #2006, .T. ) ;
#1761 = VECTOR ( 'NONE', #12386, 1000.000000000000000 ) ;
#1762 = ADVANCED_FACE ( 'NONE', ( #980 ), #3474, .F. ) ;
#1763 = DIRECTION ( 'NONE',  ( 0.000000000000000000, 0.000000000000000000, 1.000000000000000000 ) ) ;
#1764 = ADVANCED_FACE ( 'NONE', ( #7325 ), #15401, .T. ) ;
#1765 = EDGE_CURVE ( 'NONE', #903, #11543, #6504, .T. ) ;
#1766 = ORIENTED_EDGE ( 'NONE', *, *, #8788, .T. ) ;
#1767 = VECTOR ( 'NONE', #7199, 1000.000000000000000 ) ;
#1768 = ORIENTED_EDGE ( 'NONE', *, *, #6702, .F. ) ;
#1769 = CARTESIAN_POINT ( 'NONE',  ( -40.00000000000000711, 6.000000000000000000, -18.00000000000000355 ) ) ;
#1770 = AXIS2_PLACEMENT_3D ( 'NONE', #6530, #11967, #291 ) ;
#1771 = FACE_OUTER_BOUND ( 'NONE', #16670, .T. ) ;
#1772 = FACE_OUTER_BOUND ( 'NONE', #16, .T. ) ;
#1773 = DIRECTION ( 'NONE',  ( 0.9999937692730440641, -0.003530072958125829961, 4.323092548925426475E-19 ) ) ;
#1774 = DIRECTION ( 'NONE',  ( -1.000000000000000000, 0.000000000000000000, -0.000000000000000000 ) ) ;
#1775 = AXIS2_PLACEMENT_3D ( 'NONE', #7876, #4957, #5131 ) ;
#1776 = CARTESIAN_POINT ( 'NONE',  ( -0.3121190734724890725, 189.5736389302157647, 37.58596727633949541 ) ) ;
#1777 = DIRECTION ( 'NONE',  ( 0.000000000000000000, 0.000000000000000000, 1.000000000000000000 ) ) ;
#1778 = DIRECTION ( 'NONE',  ( -0.000000000000000000, -0.000000000000000000, -1.000000000000000000 ) ) ;
#1779 = DIRECTION ( 'NONE',  ( 0.000000000000000000, -6.028905917052134721E-13, 1.000000000000000000 ) ) ;
#1780 = AXIS2_PLACEMENT_3D ( 'NONE', #10245, #2497, #14197 ) ;
#1781 = DIRECTION ( 'NONE',  ( 0.000000000000000000, -0.09950371902100227373, -0.9950371902099888199 ) ) ;
#1782 = SURFACE_STYLE_USAGE ( .BOTH. , #13202 ) ;
#1784 = ORIENTED_EDGE ( 'NONE', *, *, #11710, .T. ) ;
#1783 = ORIENTED_EDGE ( 'NONE', *, *, #5969, .T. ) ;
#1785 = DIRECTION ( 'NONE',  ( -0.000000000000000000, -1.000000000000000000, -0.000000000000000000 ) ) ;
#1786 = AXIS2_PLACEMENT_3D ( 'NONE', #14256, #1198, #6328 ) ;
#1787 = CARTESIAN_POINT ( 'NONE',  ( 1.116005356545072604E-12, 285.5359281317236650, 37.50626614651405788 ) ) ;
#1788 = CARTESIAN_POINT ( 'NONE',  ( -210.0000000000000000, 512.1906115401388888, 0.000000000000000000 ) ) ;
#1789 = DIRECTION ( 'NONE',  ( -1.156482317317870344E-15, 0.000000000000000000, 1.000000000000000000 ) ) ;
#1790 = ORIENTED_EDGE ( 'NONE', *, *, #806, .F. ) ;
#1791 = CONTEXT_DEPENDENT_SHAPE_REPRESENTATION ( #10723, #3027 ) ;
#1792 = DIRECTION ( 'NONE',  ( 0.000000000000000000, 0.000000000000000000, -1.000000000000000000 ) ) ;
#1793 = ORIENTED_EDGE ( 'NONE', *, *, #9295, .T. ) ;
#1794 = CARTESIAN_POINT ( 'NONE',  ( 40.00000000000000711, 8.000000000000000000, 34.99999999999997868 ) ) ;
#1795 = AXIS2_PLACEMENT_3D ( 'NONE', #8157, #16139, #16056 ) ;
#1796 = ADVANCED_FACE ( 'NONE', ( #11951 ), #1468, .F. ) ;
#1797 = DIRECTION ( 'NONE',  ( 0.000000000000000000, 0.000000000000000000, -1.000000000000000000 ) ) ;
#1798 = CARTESIAN_POINT ( 'NONE',  ( 10.00000000000000000, 341.0487089519837696, -133.5000000000032969 ) ) ;
#1799 = FACE_OUTER_BOUND ( 'NONE', #6425, .T. ) ;
#1800 = DIRECTION ( 'NONE',  ( -1.000000000000000000, -0.000000000000000000, 0.000000000000000000 ) ) ;
#1801 = ORIENTED_EDGE ( 'NONE', *, *, #2153, .F. ) ;
#1802 = ADVANCED_FACE ( 'NONE', ( #4125 ), #15974, .F. ) ;
#1803 = DIRECTION ( 'NONE',  ( 0.000000000000000000, 0.000000000000000000, -1.000000000000000000 ) ) ;
#1804 = CARTESIAN_POINT ( 'NONE',  ( -55.99999999999989342, 493.2350855268092573, -580.5705369404290650 ) ) ;
#1805 = AXIS2_PLACEMENT_3D ( 'NONE', #11292, #7501, #11381 ) ;
#1806 = CARTESIAN_POINT ( 'NONE',  ( 46.99999999999988631, 493.2350855268092573, -589.9613477082210693 ) ) ;
#1807 = ORIENTED_EDGE ( 'NONE', *, *, #1760, .T. ) ;
#1808 = PRODUCT_DEFINITION ( 'UNKNOWN', '', #5601, #51 ) ;
#1809 = LINE ( 'NONE', #12367, #4985 ) ;
#1810 = PRODUCT ( 'Part7', 'Part7', '', ( #6708 ) ) ;
#1811 = DIRECTION ( 'NONE',  ( 1.000000000000000000, 0.000000000000000000, 0.000000000000000000 ) ) ;
#1812 = VERTEX_POINT ( 'NONE', #5411 ) ;
#1813 = CARTESIAN_POINT ( 'NONE',  ( -10.00000000000000000, -1.224646799147353454E-15, 0.000000000000000000 ) ) ;
#1814 = LINE ( 'NONE', #16322, #4622 ) ;
#1815 = DIRECTION ( 'NONE',  ( -1.156482317317875275E-15, 0.000000000000000000, -1.000000000000000000 ) ) ;
#1816 = ORIENTED_EDGE ( 'NONE', *, *, #8125, .T. ) ;
#1817 = EDGE_CURVE ( 'NONE', #6348, #3860, #1048, .T. ) ;
#1818 = VECTOR ( 'NONE', #15289, 1000.000000000000000 ) ;
#1819 = CIRCLE ( 'NONE', #7275, 9.000000000000007105 ) ;
#1820 = DIRECTION ( 'NONE',  ( 0.000000000000000000, 1.000000000000000000, 0.000000000000000000 ) ) ;
#1821 = ORIENTED_EDGE ( 'NONE', *, *, #14733, .F. ) ;
#1822 = ORIENTED_EDGE ( 'NONE', *, *, #16704, .F. ) ;
#1823 = DIRECTION ( 'NONE',  ( 0.000000000000000000, 0.000000000000000000, 1.000000000000000000 ) ) ;
#1824 = ORIENTED_EDGE ( 'NONE', *, *, #8247, .F. ) ;
#1825 = EDGE_LOOP ( 'NONE', ( #1352, #16758, #14728, #15352 ) ) ;
#1826 = CARTESIAN_POINT ( 'NONE',  ( -49.99999999999999289, 515.4878487013597805, -606.7230258972047068 ) ) ;
#1827 = AXIS2_PLACEMENT_3D ( 'NONE', #15975, #13497, #14954 ) ;
#1828 = ORIENTED_EDGE ( 'NONE', *, *, #5741, .F. ) ;
#1829 = ADVANCED_FACE ( 'NONE', ( #14443 ), #12036, .F. ) ;
#1830 = VECTOR ( 'NONE', #16891, 1000.000000000000000 ) ;
#1831 = CYLINDRICAL_SURFACE ( 'NONE', #16503, 2.999999999999999112 ) ;
#1832 = CARTESIAN_POINT ( 'NONE',  ( 0.000000000000000000, 258.8496290447203592, 286.9685381829918924 ) ) ;
#1833 = EDGE_LOOP ( 'NONE', ( #5101, #674, #2755, #13871, #16472, #6204, #15110, #16079 ) ) ;
#1834 = FACE_OUTER_BOUND ( 'NONE', #5360, .T. ) ;
#1835 = DIRECTION ( 'NONE',  ( -0.000000000000000000, -1.000000000000000000, -0.000000000000000000 ) ) ;
#1836 = ORIENTED_EDGE ( 'NONE', *, *, #4867, .F. ) ;
#1837 = EDGE_CURVE ( 'NONE', #14282, #13693, #511, .T. ) ;
#1838 = PLANE ( 'NONE',  #9977 ) ;
#1839 = VERTEX_POINT ( 'NONE', #9283 ) ;
#1840 = CARTESIAN_POINT ( 'NONE',  ( 0.000000000000000000, 425.7506394335853201, 109.9999999999999858 ) ) ;
#1841 = ORIENTED_EDGE ( 'NONE', *, *, #16639, .F. ) ;
#1842 = EDGE_LOOP ( 'NONE', ( #8254, #8543, #10834, #15114 ) ) ;
#1843 =( NAMED_UNIT ( * ) PLANE_ANGLE_UNIT ( ) SI_UNIT ( $, .RADIAN. ) );
#1844 = LINE ( 'NONE', #10861, #12501 ) ;
#1845 = ORIENTED_EDGE ( 'NONE', *, *, #4685, .F. ) ;
#1846 = ORIENTED_EDGE ( 'NONE', *, *, #9828, .T. ) ;
#1847 = CARTESIAN_POINT ( 'NONE',  ( -39.99999999999997868, 3.000000000000000000, -25.99999999999999645 ) ) ;
#1848 = EDGE_CURVE ( 'NONE', #10672, #10225, #16132, .T. ) ;
#1849 = DIRECTION ( 'NONE',  ( 0.000000000000000000, -0.8660254037844363761, -0.5000000000000039968 ) ) ;
#1850 = CARTESIAN_POINT ( 'NONE',  ( 414.6791312654406738, 352.3556387948262341, -6.736600000000000144 ) ) ;
#1851 = VECTOR ( 'NONE', #11286, 1000.000000000000000 ) ;
#1852 = DIRECTION ( 'NONE',  ( 0.000000000000000000, -1.000000000000000000, 0.000000000000000000 ) ) ;
#1853 = FACE_OUTER_BOUND ( 'NONE', #63, .T. ) ;
#1854 = EDGE_CURVE ( 'NONE', #3376, #11568, #3252, .T. ) ;
#1855 = EDGE_CURVE ( 'NONE', #14215, #544, #2145, .T. ) ;
#1856 = ADVANCED_FACE ( 'NONE', ( #9208 ), #9, .T. ) ;
#1857 = CARTESIAN_POINT ( 'NONE',  ( 55.99999999999989342, 549.5810598491746077, -518.1154249974242703 ) ) ;
#1858 = EDGE_CURVE ( 'NONE', #8348, #13693, #5487, .T. ) ;
#1859 = DIRECTION ( 'NONE',  ( -1.000000000000000000, 0.000000000000000000, 0.000000000000000000 ) ) ;
#1860 = DIRECTION ( 'NONE',  ( 1.000000000000000000, 0.000000000000000000, 0.000000000000000000 ) ) ;
#1861 = CARTESIAN_POINT ( 'NONE',  ( -26.00000000000002842, 3.000000000000000000, -31.00000000000003197 ) ) ;
#1862 = DIRECTION ( 'NONE',  ( -1.000000000000000000, 0.000000000000000000, 0.000000000000000000 ) ) ;
#1863 = CARTESIAN_POINT ( 'NONE',  ( 10.00000000000000000, 309.2289037985885898, -79.88019484660914316 ) ) ;
#1865 = VERTEX_POINT ( 'NONE', #7896 ) ;
#1864 = ORIENTED_EDGE ( 'NONE', *, *, #5398, .T. ) ;
#1866 = VECTOR ( 'NONE', #11670, 1000.000000000000000 ) ;
#1867 = CARTESIAN_POINT ( 'NONE',  ( -1.734723475976807094E-15, 60.00000000000000711, 6.000000000000000000 ) ) ;
#1868 = CARTESIAN_POINT ( 'NONE',  ( 46.99999999999988631, 523.2161522479893847, -595.2478186815853860 ) ) ;
#1869 = DIRECTION ( 'NONE',  ( -1.000000000000000000, 0.000000000000000000, -0.000000000000000000 ) ) ;
#1870 = VERTEX_POINT ( 'NONE', #10832 ) ;
#1871 = DIRECTION ( 'NONE',  ( 1.000000000000000000, 0.000000000000000000, 0.000000000000000000 ) ) ;
#1872 = ORIENTED_EDGE ( 'NONE', *, *, #14130, .F. ) ;
#1873 = DIRECTION ( 'NONE',  ( 0.000000000000000000, -0.000000000000000000, -1.000000000000000000 ) ) ;
#1874 = ADVANCED_FACE ( 'NONE', ( #13238, #5583 ), #14700, .F. ) ;
#1875 = VECTOR ( 'NONE', #7237, 1000.000000000000000 ) ;
#1876 = LINE ( 'NONE', #16548, #14994 ) ;
#1877 = DIRECTION ( 'NONE',  ( -1.000000000000000000, 3.424802208873653704E-15, 9.473616975916768164E-35 ) ) ;
#1878 = CARTESIAN_POINT ( 'NONE',  ( 55.99999999999989342, 493.2350855268086320, -508.1801094700848580 ) ) ;
#1879 = VERTEX_POINT ( 'NONE', #15718 ) ;
#1880 = CARTESIAN_POINT ( 'NONE',  ( 31.81980515339464333, 0.000000000000000000, -28.51980515339463906 ) ) ;
#1881 = CARTESIAN_POINT ( 'NONE',  ( 0.000000000000000000, 66.00000000000000000, 0.9999999999999958922 ) ) ;
#1882 = CIRCLE ( 'NONE', #11473, 59.99999999999994316 ) ;
#1883 = SHAPE_REPRESENTATION ( 'Part6', ( #1488 ), #16030 ) ;
#1884 = SURFACE_SIDE_STYLE ('',( #12200 ) ) ;
#1885 = ORIENTED_EDGE ( 'NONE', *, *, #6312, .T. ) ;
#1886 = DIRECTION ( 'NONE',  ( 0.000000000000000000, 0.000000000000000000, -1.000000000000000000 ) ) ;
#1887 = CARTESIAN_POINT ( 'NONE',  ( 39.72345254347677468, 303.2115381654813859, 0.000000000000000000 ) ) ;
#1888 = ORIENTED_EDGE ( 'NONE', *, *, #3346, .F. ) ;
#1889 = FACE_OUTER_BOUND ( 'NONE', #14706, .T. ) ;
#1890 = FACE_OUTER_BOUND ( 'NONE', #15812, .T. ) ;
#1891 = CARTESIAN_POINT ( 'NONE',  ( 37.00000000000000000, 0.000000000000000000, -23.00000000000000000 ) ) ;
#1892 = ORIENTED_EDGE ( 'NONE', *, *, #1395, .T. ) ;
#1893 = FILL_AREA_STYLE_COLOUR ( '', #14103 ) ;
#1894 = ORIENTED_EDGE ( 'NONE', *, *, #14775, .F. ) ;
#1895 = ORIENTED_EDGE ( 'NONE', *, *, #13793, .T. ) ;
#1896 = DIRECTION ( 'NONE',  ( 0.000000000000000000, -1.000000000000000000, 0.000000000000000000 ) ) ;
#1897 = APPLICATION_PROTOCOL_DEFINITION ( 'draft international standard', 'automotive_design', 1998, #10935 ) ;
#1898 = VECTOR ( 'NONE', #402, 1000.000000000000000 ) ;
#1899 = VERTEX_POINT ( 'NONE', #14521 ) ;
#1900 = CARTESIAN_POINT ( 'NONE',  ( 35.00000000000000711, 19.00000000000000000, -21.00000000000000355 ) ) ;
#1901 = ORIENTED_EDGE ( 'NONE', *, *, #14116, .T. ) ;
#1902 = DIRECTION ( 'NONE',  ( -0.000000000000000000, 1.000000000000000000, -0.000000000000000000 ) ) ;
#1903 = CARTESIAN_POINT ( 'NONE',  ( 0.000000000000000000, 66.00000000000000000, -9.500000000000000000 ) ) ;
#1904 = ORIENTED_EDGE ( 'NONE', *, *, #7512, .T. ) ;
#1905 = DIRECTION ( 'NONE',  ( -1.000000000000000000, -0.000000000000000000, -0.000000000000000000 ) ) ;
#1906 = CARTESIAN_POINT ( 'NONE',  ( 35.00000000000003553, 0.000000000000000000, -20.99999999999999645 ) ) ;
#1907 = ORIENTED_EDGE ( 'NONE', *, *, #12877, .F. ) ;
#1908 = LINE ( 'NONE', #9991, #10254 ) ;
#1909 = ORIENTED_EDGE ( 'NONE', *, *, #12976, .F. ) ;
#1910 = PLANE ( 'NONE',  #12161 ) ;
#1911 = VERTEX_POINT ( 'NONE', #1377 ) ;
#1912 = ADVANCED_FACE ( 'NONE', ( #4048 ), #2932, .F. ) ;
#1913 = EDGE_LOOP ( 'NONE', ( #2347, #2376, #16429, #15235 ) ) ;
#1914 =( NAMED_UNIT ( * ) SI_UNIT ( $, .STERADIAN. ) SOLID_ANGLE_UNIT ( ) );
#1915 = ORIENTED_EDGE ( 'NONE', *, *, #6592, .T. ) ;
#1916 = EDGE_CURVE ( 'NONE', #14044, #11373, #9366, .T. ) ;
#1917 = VECTOR ( 'NONE', #12260, 1000.000000000000000 ) ;
#1918 = EDGE_LOOP ( 'NONE', ( #6102, #11356, #4647, #15464 ) ) ;
#1919 = CARTESIAN_POINT ( 'NONE',  ( -0.9699764831012689381, 38.15427877784792088, 9.452135968713491820 ) ) ;
#1920 = VECTOR ( 'NONE', #1030, 1000.000000000000000 ) ;
#1921 = DIRECTION ( 'NONE',  ( 1.000000000000000000, 0.000000000000000000, 0.000000000000000000 ) ) ;
#1922 = CARTESIAN_POINT ( 'NONE',  ( 56.72999999999999687, 189.4632308570086536, 37.52989836422092651 ) ) ;
#1923 = CARTESIAN_POINT ( 'NONE',  ( 46.99999999999988631, 493.2350855268086320, -508.1801094700848580 ) ) ;
#1924 = PRODUCT_DEFINITION_SHAPE ( 'NONE', 'NONE',  #16970 ) ;
#1925 = DIRECTION ( 'NONE',  ( 0.000000000000000000, 1.000000000000000000, 0.000000000000000000 ) ) ;
#1926 = DIRECTION ( 'NONE',  ( 0.000000000000000000, 0.000000000000000000, -1.000000000000000000 ) ) ;
#1927 = DIRECTION ( 'NONE',  ( 0.000000000000000000, -1.000000000000000000, 2.220446049250308742E-15 ) ) ;
#1928 = ORIENTED_EDGE ( 'NONE', *, *, #12665, .F. ) ;
#1929 = DIRECTION ( 'NONE',  ( 0.000000000000000000, 1.000000000000000000, 0.000000000000000000 ) ) ;
#1930 = FACE_OUTER_BOUND ( 'NONE', #6718, .T. ) ;
#1931 = CIRCLE ( 'NONE', #7397, 13.69540538389601991 ) ;
#1932 = EDGE_CURVE ( 'NONE', #14417, #11237, #9548, .T. ) ;
#1933 = VECTOR ( 'NONE', #15848, 1000.000000000000000 ) ;
#1934 = LINE ( 'NONE', #573, #6396 ) ;
#1935 = CARTESIAN_POINT ( 'NONE',  ( -40.00000000000000000, 68.00000000000000000, -25.99999999999999645 ) ) ;
#1937 = ORIENTED_EDGE ( 'NONE', *, *, #3285, .F. ) ;
#1936 = ORIENTED_EDGE ( 'NONE', *, *, #5116, .T. ) ;
#1938 = LINE ( 'NONE', #4928, #6715 ) ;
#1939 = EDGE_CURVE ( 'NONE', #6725, #11290, #5326, .T. ) ;
#1940 = ADVANCED_FACE ( 'NONE', ( #1890 ), #10999, .T. ) ;
#1941 = SURFACE_STYLE_USAGE ( .BOTH. , #11218 ) ;
#1942 = EDGE_CURVE ( 'NONE', #5920, #13660, #4708, .T. ) ;
#1943 = DIRECTION ( 'NONE',  ( 0.000000000000000000, 1.000000000000000000, 0.000000000000000000 ) ) ;
#1944 = FACE_OUTER_BOUND ( 'NONE', #14445, .T. ) ;
#1945 = AXIS2_PLACEMENT_3D ( 'NONE', #5289, #15378, #3613 ) ;
#1946 = VERTEX_POINT ( 'NONE', #12209 ) ;
#1947 = LINE ( 'NONE', #508, #740 ) ;
#1948 = VERTEX_POINT ( 'NONE', #3268 ) ;
#1949 = CARTESIAN_POINT ( 'NONE',  ( -2.844883903241206546, 60.97223153686513086, 9.064373830433188672 ) ) ;
#1950 = CARTESIAN_POINT ( 'NONE',  ( 0.2839248860676515940, 192.8804468505487932, 37.35595106346518435 ) ) ;
#1951 = LINE ( 'NONE', #4783, #6081 ) ;
#1952 = CARTESIAN_POINT ( 'NONE',  ( 22.99999999999999645, 68.00000000000000000, 31.00000000000006750 ) ) ;
#1953 = CARTESIAN_POINT ( 'NONE',  ( 31.00000000000001421, 10.00000000000000000, 22.99999999999999645 ) ) ;
#1954 = VERTEX_POINT ( 'NONE', #1970 ) ;
#1955 = AXIS2_PLACEMENT_3D ( 'NONE', #7847, #15843, #13107 ) ;
#1956 = CARTESIAN_POINT ( 'NONE',  ( 0.000000000000000000, -3.000000000000000000, -18.50000000000000000 ) ) ;
#1957 = ADVANCED_FACE ( 'NONE', ( #9966 ), #1723, .F. ) ;
#1958 = EDGE_CURVE ( 'NONE', #3705, #9126, #12039, .T. ) ;
#1959 = DIRECTION ( 'NONE',  ( 0.000000000000000000, 0.000000000000000000, 1.000000000000000000 ) ) ;
#1960 = EDGE_CURVE ( 'NONE', #14037, #7396, #11760, .T. ) ;
#1961 = VECTOR ( 'NONE', #13730, 1000.000000000000000 ) ;
#1962 = CIRCLE ( 'NONE', #1695, 18.50000000000000000 ) ;
#1963 = CARTESIAN_POINT ( 'NONE',  ( -46.99999999999988631, 473.6663340069158039, -561.9448123979092315 ) ) ;
#1964 = VERTEX_POINT ( 'NONE', #7035 ) ;
#1965 = LINE ( 'NONE', #7280, #12674 ) ;
#1966 = VECTOR ( 'NONE', #10588, 1000.000000000000000 ) ;
#1967 = DIRECTION ( 'NONE',  ( -1.000000000000000000, 0.000000000000000000, -0.000000000000000000 ) ) ;
#1968 = ORIENTED_EDGE ( 'NONE', *, *, #6535, .F. ) ;
#1969 = CYLINDRICAL_SURFACE ( 'NONE', #1212, 8.000000000000000000 ) ;
#1970 = CARTESIAN_POINT ( 'NONE',  ( 40.00000000000000711, 11.00000000000000000, 25.99999999999999645 ) ) ;
#1971 = DIRECTION ( 'NONE',  ( 0.000000000000000000, 0.000000000000000000, 1.000000000000000000 ) ) ;
#1972 = ORIENTED_EDGE ( 'NONE', *, *, #16844, .T. ) ;
#1973 = ADVANCED_BREP_SHAPE_REPRESENTATION ( '', ( #2742, #1488 ), #4776 ) ;
#1974 = VECTOR ( 'NONE', #10387, 1000.000000000000000 ) ;
#1975 = LINE ( 'NONE', #783, #15475 ) ;
#1976 = AXIS2_PLACEMENT_3D ( 'NONE', #7527, #16886, #13122 ) ;
#1977 = VERTEX_POINT ( 'NONE', #3189 ) ;
#1978 = VERTEX_POINT ( 'NONE', #7196 ) ;
#1979 = FACE_OUTER_BOUND ( 'NONE', #16392, .T. ) ;
#1980 = APPLICATION_PROTOCOL_DEFINITION ( 'draft international standard', 'automotive_design', 1998, #3036 ) ;
#1981 = AXIS2_PLACEMENT_3D ( 'NONE', #2659, #2321, #1119 ) ;
#1982 = DIRECTION ( 'NONE',  ( 1.000000000000000000, 0.000000000000000000, 0.000000000000000000 ) ) ;
#1983 = VERTEX_POINT ( 'NONE', #3440 ) ;
#1984 = AXIS2_PLACEMENT_3D ( 'NONE', #1158, #11386, #15418 ) ;
#1985 = CARTESIAN_POINT ( 'NONE',  ( -55.99999999999989342, 473.6663340069158039, -561.9448123979092315 ) ) ;
#1986 = DIRECTION ( 'NONE',  ( 0.000000000000000000, 0.000000000000000000, 1.000000000000000000 ) ) ;
#1987 = EDGE_LOOP ( 'NONE', ( #15123, #3976, #13341, #8270 ) ) ;
#1988 = CARTESIAN_POINT ( 'NONE',  ( 0.000000000000000000, 240.7889724647196488, -10.68226574335980139 ) ) ;
#1989 = DIRECTION ( 'NONE',  ( -1.000000000000000000, -1.622872818267927724E-12, 1.623597793334635938E-13 ) ) ;
#1990 = ORIENTED_EDGE ( 'NONE', *, *, #11512, .T. ) ;
#1991 = CIRCLE ( 'NONE', #2538, 7.500000000000000000 ) ;
#1992 = CARTESIAN_POINT ( 'NONE',  ( 394.0000000000001137, 339.1725919290087745, -9.945665743359786148 ) ) ;
#1993 = EDGE_CURVE ( 'NONE', #6752, #5994, #15031, .T. ) ;
#1994 = ORIENTED_EDGE ( 'NONE', *, *, #12802, .F. ) ;
#1995 = VERTEX_POINT ( 'NONE', #8679 ) ;
#1996 = VECTOR ( 'NONE', #9358, 1000.000000000000000 ) ;
#1997 = EDGE_LOOP ( 'NONE', ( #12559, #322, #14053, #5318 ) ) ;
#1998 = EDGE_CURVE ( 'NONE', #15577, #2365, #12290, .T. ) ;
#1999 = ORIENTED_EDGE ( 'NONE', *, *, #8965, .T. ) ;
#2000 = AXIS2_PLACEMENT_3D ( 'NONE', #13436, #6879, #12137 ) ;
#2001 = ORIENTED_EDGE ( 'NONE', *, *, #14775, .T. ) ;
#2002 = LINE ( 'NONE', #1769, #5254 ) ;
#2003 = CARTESIAN_POINT ( 'NONE',  ( -23.00000000000002132, 6.000000000000000000, 32.00000000000000000 ) ) ;
#2004 = LINE ( 'NONE', #7236, #6944 ) ;
#2005 = EDGE_CURVE ( 'NONE', #12856, #6207, #14791, .T. ) ;
#2006 = LINE ( 'NONE', #12747, #1875 ) ;
#2007 = AXIS2_PLACEMENT_3D ( 'NONE', #15258, #12676, #6137 ) ;
#2008 = CARTESIAN_POINT ( 'NONE',  ( -20.99999999999999645, 19.00000000000000000, -31.00000000000003908 ) ) ;
#2009 = CARTESIAN_POINT ( 'NONE',  ( 0.000000000000000000, 8.000000000000000000, 0.000000000000000000 ) ) ;
#2010 = CARTESIAN_POINT ( 'NONE',  ( 39.72345254347677468, 303.2115381654813859, -10.00000000000000000 ) ) ;
#2011 = ORIENTED_EDGE ( 'NONE', *, *, #10862, .F. ) ;
#2012 = LINE ( 'NONE', #16190, #16374 ) ;
#2013 = FACE_OUTER_BOUND ( 'NONE', #11234, .T. ) ;
#2014 = CIRCLE ( 'NONE', #11610, 13.69540538389601991 ) ;
#2015 = EDGE_CURVE ( 'NONE', #7006, #11353, #1814, .T. ) ;
#2016 = CARTESIAN_POINT ( 'NONE',  ( 22.99999999999998224, 6.000000000000000000, -31.00000000000003197 ) ) ;
#2017 = LINE ( 'NONE', #12333, #11515 ) ;
#2019 = ORIENTED_EDGE ( 'NONE', *, *, #11303, .T. ) ;
#2018 = ORIENTED_EDGE ( 'NONE', *, *, #13805, .F. ) ;
#2020 = CARTESIAN_POINT ( 'NONE',  ( -39.99999999999999289, 11.00000000000000000, -26.00000000000000355 ) ) ;
#2021 =( GEOMETRIC_REPRESENTATION_CONTEXT ( 3 ) GLOBAL_UNCERTAINTY_ASSIGNED_CONTEXT ( ( #12027 ) ) GLOBAL_UNIT_ASSIGNED_CONTEXT ( ( #12468, #710, #9979 ) ) REPRESENTATION_CONTEXT ( 'NONE', 'WORKASPACE' ) );
#2022 = AXIS2_PLACEMENT_3D ( 'NONE', #6899, #13453, #1415 ) ;
#2023 = ORIENTED_EDGE ( 'NONE', *, *, #535, .F. ) ;
#2024 = AXIS2_PLACEMENT_3D ( 'NONE', #4522, #3238, #11129 ) ;
#2025 = CARTESIAN_POINT ( 'NONE',  ( -32.00000000000000711, 6.000000000000000000, -23.00000000000000000 ) ) ;
#2026 = DIRECTION ( 'NONE',  ( 0.000000000000000000, 1.000000000000000000, 0.000000000000000000 ) ) ;
#2027 = EDGE_LOOP ( 'NONE', ( #12817, #3120, #13749, #13996 ) ) ;
#2028 = EDGE_CURVE ( 'NONE', #10388, #1481, #8195, .T. ) ;
#2029 = DIRECTION ( 'NONE',  ( 0.000000000000000000, 0.000000000000000000, -1.000000000000000000 ) ) ;
#2030 = PRODUCT_DEFINITION_FORMATION_WITH_SPECIFIED_SOURCE ( 'ANY', '', #1810, .NOT_KNOWN. ) ;
#2031 = DIRECTION ( 'NONE',  ( -1.000000000000000000, 0.000000000000000000, 0.000000000000000000 ) ) ;
#2032 = ORIENTED_EDGE ( 'NONE', *, *, #6664, .T. ) ;
#2033 = CARTESIAN_POINT ( 'NONE',  ( -39.99999999999997868, -20.00000000000000000, -19.99999999999999645 ) ) ;
#2034 = VECTOR ( 'NONE', #2855, 1000.000000000000000 ) ;
#2035 = FACE_OUTER_BOUND ( 'NONE', #15996, .T. ) ;
#2036 = CARTESIAN_POINT ( 'NONE',  ( -2.220446049250313081E-13, 75.00000000000001421, 3.000000000000000000 ) ) ;
#2037 = EDGE_CURVE ( 'NONE', #7396, #884, #9721, .T. ) ;
#2038 = AXIS2_PLACEMENT_3D ( 'NONE', #7707, #1285, #6500 ) ;
#2039 = LINE ( 'NONE', #5983, #7253 ) ;
#2040 = DIRECTION ( 'NONE',  ( -1.000000000000000000, 0.000000000000000000, -0.000000000000000000 ) ) ;
#2041 = ORIENTED_EDGE ( 'NONE', *, *, #6763, .T. ) ;
#2042 = CARTESIAN_POINT ( 'NONE',  ( -30.99999999999999289, 0.000000000000000000, 31.00000000000000000 ) ) ;
#2043 = LINE ( 'NONE', #14338, #8366 ) ;
#2044 = DIRECTION ( 'NONE',  ( -0.9998870921963913805, -0.01502673813723916056, 0.000000000000000000 ) ) ;
#2045 = VERTEX_POINT ( 'NONE', #4393 ) ;
#2046 = AXIS2_PLACEMENT_3D ( 'NONE', #4775, #11301, #8655 ) ;
#2047 = FILL_AREA_STYLE_COLOUR ( '', #7195 ) ;
#2048 = ORIENTED_EDGE ( 'NONE', *, *, #15763, .T. ) ;
#2049 = EDGE_CURVE ( 'NONE', #1069, #9318, #15108, .T. ) ;
#2050 = CIRCLE ( 'NONE', #12761, 4.695405383895955964 ) ;
#2051 = EDGE_CURVE ( 'NONE', #2088, #13185, #16401, .T. ) ;
#2052 = CARTESIAN_POINT ( 'NONE',  ( 7.000000000000001776, 380.0000000000000000, -65.00000000000000000 ) ) ;
#2053 = CARTESIAN_POINT ( 'NONE',  ( -45.00000000000000000, 559.9933750504617365, -546.7230258972048205 ) ) ;
#2054 = VERTEX_POINT ( 'NONE', #14953 ) ;
#2055 = DIRECTION ( 'NONE',  ( -0.000000000000000000, -1.000000000000000000, -0.000000000000000000 ) ) ;
#2056 = ADVANCED_FACE ( 'NONE', ( #8428 ), #701, .F. ) ;
#2057 = DIRECTION ( 'NONE',  ( 0.000000000000000000, 1.000000000000000000, 0.000000000000000000 ) ) ;
#2058 = LINE ( 'NONE', #13833, #5096 ) ;
#2059 = EDGE_LOOP ( 'NONE', ( #15397, #6986, #8899, #7553, #1283 ) ) ;
#2060 = EDGE_CURVE ( 'NONE', #3345, #3903, #14866, .T. ) ;
#2061 = EDGE_CURVE ( 'NONE', #16656, #11956, #15320, .T. ) ;
#2062 = EDGE_CURVE ( 'NONE', #117, #2600, #1031, .T. ) ;
#2063 = CARTESIAN_POINT ( 'NONE',  ( -26.00000000000002132, 8.000000000000000000, 40.00000000000000711 ) ) ;
#2064 = CARTESIAN_POINT ( 'NONE',  ( 5.162501635565829972, 0.000000000000000000, 0.000000000000000000 ) ) ;
#2065 = VERTEX_POINT ( 'NONE', #10049 ) ;
#2066 = ORIENTED_EDGE ( 'NONE', *, *, #10313, .F. ) ;
#2067 = DIRECTION ( 'NONE',  ( -0.000000000000000000, 1.000000000000000000, -0.000000000000000000 ) ) ;
#2068 = CIRCLE ( 'NONE', #10575, 5.268482129199949959 ) ;
#2069 = PRODUCT_CONTEXT ( 'NONE', #628, 'mechanical' ) ;
#2070 = DIRECTION ( 'NONE',  ( -0.000000000000000000, -1.000000000000000000, -0.000000000000000000 ) ) ;
#2071 = ORIENTED_EDGE ( 'NONE', *, *, #6201, .F. ) ;
#2072 = CARTESIAN_POINT ( 'NONE',  ( -23.00000000000003197, 3.000000000000000000, 34.00000000000000711 ) ) ;
#2073 = DIRECTION ( 'NONE',  ( 0.000000000000000000, 0.000000000000000000, -1.000000000000000000 ) ) ;
#2074 = VECTOR ( 'NONE', #6098, 1000.000000000000227 ) ;
#2075 = VERTEX_POINT ( 'NONE', #15288 ) ;
#2076 = VECTOR ( 'NONE', #10731, 1000.000000000000000 ) ;
#2077 = LINE ( 'NONE', #12476, #5855 ) ;
#2078 = LINE ( 'NONE', #7384, #10309 ) ;
#2079 = EDGE_LOOP ( 'NONE', ( #12382, #14204, #2230, #959 ) ) ;
#2080 = EDGE_CURVE ( 'NONE', #5021, #4345, #3601, .T. ) ;
#2081 = PLANE ( 'NONE',  #8050 ) ;
#2082 = ORIENTED_EDGE ( 'NONE', *, *, #9538, .F. ) ;
#2083 = VERTEX_POINT ( 'NONE', #7697 ) ;
#2084 = ORIENTED_EDGE ( 'NONE', *, *, #7070, .F. ) ;
#2085 = CIRCLE ( 'NONE', #8683, 13.69540538389601991 ) ;
#2086 = CIRCLE ( 'NONE', #4557, 3.000000000000002665 ) ;
#2087 = ORIENTED_EDGE ( 'NONE', *, *, #13927, .T. ) ;
#2088 = VERTEX_POINT ( 'NONE', #8759 ) ;
#2089 = CARTESIAN_POINT ( 'NONE',  ( 25.99999999999996092, 0.000000000000000000, 31.00000000000004263 ) ) ;
#2090 = EDGE_CURVE ( 'NONE', #14834, #15661, #2391, .T. ) ;
#2091 = CARTESIAN_POINT ( 'NONE',  ( 37.00000000000003553, -20.00000000000000000, 20.00000000000000000 ) ) ;
#2092 = LINE ( 'NONE', #3473, #9439 ) ;
#2093 = LINE ( 'NONE', #16517, #16944 ) ;
#2094 = LINE ( 'NONE', #13954, #3383 ) ;
#2095 = DIRECTION ( 'NONE',  ( -1.000000000000000000, -0.000000000000000000, -0.000000000000000000 ) ) ;
#2096 = CIRCLE ( 'NONE', #11697, 22.50000000000000000 ) ;
#2097 = CARTESIAN_POINT ( 'NONE',  ( 55.99999999999989342, 523.2161522479893847, -590.5524132976893270 ) ) ;
#2098 = VECTOR ( 'NONE', #3498, 1000.000000000000000 ) ;
#2099 = CARTESIAN_POINT ( 'NONE',  ( 21.00000000000000000, 19.00000000000000000, 35.00000000000001421 ) ) ;
#2100 = ORIENTED_EDGE ( 'NONE', *, *, #6851, .F. ) ;
#2101 = CYLINDRICAL_SURFACE ( 'NONE', #14180, 18.50000000000000000 ) ;
#2102 = DIRECTION ( 'NONE',  ( 0.000000000000000000, 1.000000000000000000, 0.000000000000000000 ) ) ;
#2104 = EDGE_LOOP ( 'NONE', ( #4360, #15232, #4965, #16382 ) ) ;
#2103 = VERTEX_POINT ( 'NONE', #6077 ) ;
#2105 = LINE ( 'NONE', #11133, #2328 ) ;
#2106 = ORIENTED_EDGE ( 'NONE', *, *, #5569, .F. ) ;
#2107 = VECTOR ( 'NONE', #12581, 1000.000000000000000 ) ;
#2108 = CONICAL_SURFACE ( 'NONE', #9492, 14.92500000000000071, 1.076854957875310381 ) ;
#2109 = CARTESIAN_POINT ( 'NONE',  ( -19.00000000000001776, 8.000000000000000000, 40.00000000000000711 ) ) ;
#2110 = CARTESIAN_POINT ( 'NONE',  ( -31.00000000000007105, 10.00000000000000000, 23.00000000000000000 ) ) ;
#2111 = ORIENTED_EDGE ( 'NONE', *, *, #15800, .F. ) ;
#2112 = UNCERTAINTY_MEASURE_WITH_UNIT (LENGTH_MEASURE( 1.000000000000000082E-05 ), #15978, 'distance_accuracy_value', 'NONE');
#2113 = LINE ( 'NONE', #12593, #14387 ) ;
#2114 = DIRECTION ( 'NONE',  ( -1.000000000000000000, -0.000000000000000000, -0.000000000000000000 ) ) ;
#2115 = ORIENTED_EDGE ( 'NONE', *, *, #9611, .F. ) ;
#2116 = CARTESIAN_POINT ( 'NONE',  ( -2.903217335657449993, 60.78097370076725525, 9.045605051663343943 ) ) ;
#2117 = CARTESIAN_POINT ( 'NONE',  ( 1.391674230819584651E-12, 193.3905335822941538, 37.50626614651405788 ) ) ;
#2118 = DIRECTION ( 'NONE',  ( 0.000000000000000000, -1.000000000000000000, 0.000000000000000000 ) ) ;
#2119 = VECTOR ( 'NONE', #14940, 1000.000000000000000 ) ;
#2120 = CYLINDRICAL_SURFACE ( 'NONE', #4529, 4.000000000000003553 ) ;
#2121 = CARTESIAN_POINT ( 'NONE',  ( 55.99999999999989342, 523.2161522479893847, -590.5524132976893270 ) ) ;
#2122 = ORIENTED_EDGE ( 'NONE', *, *, #15669, .T. ) ;
#2123 = DIRECTION ( 'NONE',  ( -1.000000000000000000, -0.000000000000000000, -0.000000000000000000 ) ) ;
#2124 = EDGE_CURVE ( 'NONE', #15922, #4232, #4803, .T. ) ;
#2125 = ADVANCED_FACE ( 'NONE', ( #16809 ), #11666, .T. ) ;
#2126 = DIRECTION ( 'NONE',  ( -1.000000000000000000, 0.000000000000000000, 0.000000000000000000 ) ) ;
#2127 = ORIENTED_EDGE ( 'NONE', *, *, #2167, .F. ) ;
#2128 = CARTESIAN_POINT ( 'NONE',  ( 21.00000000000000000, 19.00000000000000000, 35.00000000000001421 ) ) ;
#2129 = VECTOR ( 'NONE', #7523, 1000.000000000000000 ) ;
#2130 = EDGE_CURVE ( 'NONE', #14532, #3723, #16651, .T. ) ;
#2131 = ORIENTED_EDGE ( 'NONE', *, *, #15166, .T. ) ;
#2132 = DIRECTION ( 'NONE',  ( 1.000000000000000000, -0.000000000000000000, 0.000000000000000000 ) ) ;
#2133 = DIRECTION ( 'NONE',  ( -1.000000000000000000, 0.000000000000000000, -0.000000000000000000 ) ) ;
#2134 = ORIENTED_EDGE ( 'NONE', *, *, #3086, .F. ) ;
#2135 = FACE_OUTER_BOUND ( 'NONE', #12376, .T. ) ;
#2136 = CARTESIAN_POINT ( 'NONE',  ( -55.99999999999989342, 473.6663340069158039, -561.9448123979092315 ) ) ;
#2137 = LINE ( 'NONE', #12616, #11139 ) ;
#2138 = ORIENTED_EDGE ( 'NONE', *, *, #5649, .T. ) ;
#2139 = DIRECTION ( 'NONE',  ( -1.000000000000000000, -0.000000000000000000, 3.854941057726247958E-16 ) ) ;
#2140 = DIRECTION ( 'NONE',  ( 1.000000000000000000, 0.000000000000000000, 0.000000000000000000 ) ) ;
#2141 = ORIENTED_EDGE ( 'NONE', *, *, #7590, .F. ) ;
#2142 = VERTEX_POINT ( 'NONE', #13994 ) ;
#2143 = LINE ( 'NONE', #5846, #15483 ) ;
#2144 = EDGE_CURVE ( 'NONE', #8672, #11801, #12615, .T. ) ;
#2145 = CIRCLE ( 'NONE', #2409, 13.69540538389601991 ) ;
#2146 = SHAPE_DEFINITION_REPRESENTATION ( #8090, #12316 ) ;
#2147 = APPLICATION_CONTEXT ( 'automotive_design' ) ;
#2148 = SHAPE_REPRESENTATION_RELATIONSHIP ( 'NONE' , 'NONE' ,  #12316, #11622 ) ;
#2149 = EDGE_CURVE ( 'NONE', #529, #5229, #12793, .T. ) ;
#2150 = DIRECTION ( 'NONE',  ( -0.000000000000000000, 0.000000000000000000, 1.000000000000000000 ) ) ;
#2151 = EDGE_CURVE ( 'NONE', #16324, #5994, #12953, .T. ) ;
#2152 = ORIENTED_EDGE ( 'NONE', *, *, #890, .T. ) ;
#2153 = EDGE_CURVE ( 'NONE', #14413, #13380, #15617, .T. ) ;
#2154 = DIRECTION ( 'NONE',  ( -1.000000000000000000, -0.000000000000000000, -0.000000000000000000 ) ) ;
#2155 = LINE ( 'NONE', #6423, #939 ) ;
#2156 = ORIENTED_EDGE ( 'NONE', *, *, #14025, .F. ) ;
#2157 = CARTESIAN_POINT ( 'NONE',  ( 55.99999999999989342, 493.2350855268086320, -508.1801094700848580 ) ) ;
#2158 = VECTOR ( 'NONE', #14746, 1000.000000000000000 ) ;
#2159 = CARTESIAN_POINT ( 'NONE',  ( 394.0000000000001137, 339.3157724647196005, -10.68226574335978718 ) ) ;
#2160 = EDGE_LOOP ( 'NONE', ( #3106, #13738, #4544, #14107 ) ) ;
#2161 = PRESENTATION_STYLE_ASSIGNMENT (( #8706 ) ) ;
#2162 = VERTEX_POINT ( 'NONE', #10130 ) ;
#2163 = ORIENTED_EDGE ( 'NONE', *, *, #4790, .T. ) ;
#2164 = VERTEX_POINT ( 'NONE', #3854 ) ;
#2165 = PRODUCT ( 'Part3', 'Part3', '', ( #7454 ) ) ;
#2166 = ORIENTED_EDGE ( 'NONE', *, *, #8686, .F. ) ;
#2167 = EDGE_CURVE ( 'NONE', #365, #8443, #7444, .T. ) ;
#2168 = ADVANCED_FACE ( 'NONE', ( #9014 ), #16569, .T. ) ;
#2169 = ORIENTED_EDGE ( 'NONE', *, *, #11404, .T. ) ;
#2170 = FACE_OUTER_BOUND ( 'NONE', #11247, .T. ) ;
#2171 = ADVANCED_FACE ( 'NONE', ( #12707, #945 ), #6165, .F. ) ;
#2172 = CARTESIAN_POINT ( 'NONE',  ( 25.99999999999996092, 0.000000000000000000, 40.00000000000000711 ) ) ;
#2173 = CARTESIAN_POINT ( 'NONE',  ( 0.000000000000000000, 339.3157724647196005, -104.9456657433597968 ) ) ;
#2174 = CIRCLE ( 'NONE', #14527, 4.999999999999997335 ) ;
#2175 = DIRECTION ( 'NONE',  ( 1.141265444721583757E-16, -1.000000000000000000, 0.000000000000000000 ) ) ;
#2176 = LINE ( 'NONE', #6275, #6647 ) ;
#2177 = PLANE ( 'NONE',  #3938 ) ;
#2178 = CARTESIAN_POINT ( 'NONE',  ( 55.99999999999989342, 549.5810598491749488, -575.3306267969850296 ) ) ;
#2179 = FACE_BOUND ( 'NONE', #1095, .T. ) ;
#2180 = ORIENTED_EDGE ( 'NONE', *, *, #15459, .F. ) ;
#2181 = LINE ( 'NONE', #16524, #10342 ) ;
#2182 = CARTESIAN_POINT ( 'NONE',  ( -45.00000000000000000, 559.9933750504617365, -533.0276205133087615 ) ) ;
#2183 = ADVANCED_BREP_SHAPE_REPRESENTATION ( '', ( #14480, #1488 ), #15199 ) ;
#2184 = DIRECTION ( 'NONE',  ( 1.000000000000000000, 0.000000000000000000, 0.000000000000000000 ) ) ;
#2185 = EDGE_CURVE ( 'NONE', #10598, #974, #14079, .T. ) ;
#2187 = ORIENTED_EDGE ( 'NONE', *, *, #7604, .T. ) ;
#2186 = ORIENTED_EDGE ( 'NONE', *, *, #2130, .F. ) ;
#2188 = DIRECTION ( 'NONE',  ( 1.000000000000000000, -0.000000000000000000, 0.000000000000000000 ) ) ;
#2189 = AXIS2_PLACEMENT_3D ( 'NONE', #9421, #14751, #13550 ) ;
#2190 = VECTOR ( 'NONE', #1255, 1000.000000000000000 ) ;
#2191 = ORIENTED_EDGE ( 'NONE', *, *, #2269, .F. ) ;
#2192 = DIRECTION ( 'NONE',  ( 0.000000000000000000, 0.000000000000000000, -1.000000000000000000 ) ) ;
#2193 = CARTESIAN_POINT ( 'NONE',  ( -25.99999999999999645, 68.00000000000000000, 31.00000000000003908 ) ) ;
#2194 = DIRECTION ( 'NONE',  ( 0.000000000000000000, 0.000000000000000000, 1.000000000000000000 ) ) ;
#2195 = ORIENTED_EDGE ( 'NONE', *, *, #7824, .F. ) ;
#2196 = DIRECTION ( 'NONE',  ( -0.000000000000000000, -1.000000000000000000, -0.000000000000000000 ) ) ;
#2197 = CIRCLE ( 'NONE', #9618, 13.69540538389601991 ) ;
#2198 = CYLINDRICAL_SURFACE ( 'NONE', #12808, 60.00000000000000000 ) ;
#2199 = ORIENTED_EDGE ( 'NONE', *, *, #1502, .T. ) ;
#2200 = FACE_OUTER_BOUND ( 'NONE', #246, .T. ) ;
#2201 = VECTOR ( 'NONE', #2370, 1000.000000000000000 ) ;
#2202 = DIRECTION ( 'NONE',  ( 0.000000000000000000, 0.000000000000000000, -1.000000000000000000 ) ) ;
#2203 = FACE_OUTER_BOUND ( 'NONE', #787, .T. ) ;
#2204 = CARTESIAN_POINT ( 'NONE',  ( -1.141714397801704670E-14, 289.4632308570086252, 37.52989836422091230 ) ) ;
#2205 = LINE ( 'NONE', #10035, #3242 ) ;
#2206 = ORIENTED_EDGE ( 'NONE', *, *, #6634, .T. ) ;
#2207 = DIRECTION ( 'NONE',  ( -0.000000000000000000, -0.000000000000000000, 1.000000000000000000 ) ) ;
#2208 = AXIS2_PLACEMENT_3D ( 'NONE', #8137, #1943, #9522 ) ;
#2209 = CARTESIAN_POINT ( 'NONE',  ( 25.99999999999996092, 3.000000000000000000, -31.00000000000003197 ) ) ;
#2210 = DIRECTION ( 'NONE',  ( -0.000000000000000000, 0.000000000000000000, -1.000000000000000000 ) ) ;
#2211 = ORIENTED_EDGE ( 'NONE', *, *, #870, .F. ) ;
#2212 = CARTESIAN_POINT ( 'NONE',  ( -35.00000000000000000, 19.00000000000000000, 20.99999999999999289 ) ) ;
#2213 = PRODUCT_DEFINITION ( 'UNKNOWN', '', #2030, #16147 ) ;
#2214 = CARTESIAN_POINT ( 'NONE',  ( 10.00000000000000000, 309.2289037985885898, -83.18019484660915452 ) ) ;
#2215 = ORIENTED_EDGE ( 'NONE', *, *, #16948, .T. ) ;
#2216 = DIRECTION ( 'NONE',  ( -1.000000000000000000, 0.000000000000000000, 1.156482317317875472E-15 ) ) ;
#2217 = DIRECTION ( 'NONE',  ( -0.000000000000000000, -0.000000000000000000, 1.000000000000000000 ) ) ;
#2218 = CARTESIAN_POINT ( 'NONE',  ( 0.000000000000000000, 0.000000000000000000, 3.000000000000000000 ) ) ;
#2219 = ORIENTED_EDGE ( 'NONE', *, *, #10037, .T. ) ;
#2220 = AXIS2_PLACEMENT_3D ( 'NONE', #6030, #13775, #6194 ) ;
#2221 = SURFACE_STYLE_FILL_AREA ( #3525 ) ;
#2222 = DIRECTION ( 'NONE',  ( 0.000000000000000000, 0.000000000000000000, 1.000000000000000000 ) ) ;
#2223 = FACE_OUTER_BOUND ( 'NONE', #4703, .T. ) ;
#2224 = ORIENTED_EDGE ( 'NONE', *, *, #15592, .F. ) ;
#2225 = EDGE_CURVE ( 'NONE', #9633, #11217, #5440, .T. ) ;
#2226 = DIRECTION ( 'NONE',  ( -0.000000000000000000, 1.000000000000000000, -0.000000000000000000 ) ) ;
#2227 = PRODUCT_CONTEXT ( 'NONE', #4459, 'mechanical' ) ;
#2228 = FACE_OUTER_BOUND ( 'NONE', #10422, .T. ) ;
#2229 = AXIS2_PLACEMENT_3D ( 'NONE', #14202, #13086, #3985 ) ;
#2230 = ORIENTED_EDGE ( 'NONE', *, *, #7181, .T. ) ;
#2231 = DIRECTION ( 'NONE',  ( 0.000000000000000000, 0.000000000000000000, -1.000000000000000000 ) ) ;
#2232 = CARTESIAN_POINT ( 'NONE',  ( -3.000000000000000000, -1.836909530733565148E-16, 3.000000000000000000 ) ) ;
#2233 = CIRCLE ( 'NONE', #12940, 13.69540538389596485 ) ;
#2234 = EDGE_CURVE ( 'NONE', #12483, #4508, #16959, .T. ) ;
#2235 = VERTEX_POINT ( 'NONE', #12256 ) ;
#2236 = CARTESIAN_POINT ( 'NONE',  ( 415.0210210471910841, 329.6061121441327941, -6.736600000000000144 ) ) ;
#2237 = VECTOR ( 'NONE', #1349, 1000.000000000000000 ) ;
#2238 = ADVANCED_FACE ( 'NONE', ( #10878 ), #14329, .F. ) ;
#2239 = CARTESIAN_POINT ( 'NONE',  ( -40.00000000000000000, 19.00000000000000000, -26.00000000000000355 ) ) ;
#2240 = EDGE_LOOP ( 'NONE', ( #4765, #9169, #16586, #8598, #11088, #1134, #16842, #10933, #16427, #4181, #14712, #10577, #7465, #12643, #6008, #16320 ) ) ;
#2241 = LINE ( 'NONE', #7640, #658 ) ;
#2242 = EDGE_CURVE ( 'NONE', #9686, #1196, #490, .T. ) ;
#2243 = VERTEX_POINT ( 'NONE', #16280 ) ;
#2244 = ORIENTED_EDGE ( 'NONE', *, *, #9228, .T. ) ;
#2245 = AXIS2_PLACEMENT_3D ( 'NONE', #10314, #10395, #9199 ) ;
#2246 = EDGE_CURVE ( 'NONE', #7889, #13660, #2561, .T. ) ;
#2247 = EDGE_CURVE ( 'NONE', #16075, #1365, #13374, .T. ) ;
#2248 = ORIENTED_EDGE ( 'NONE', *, *, #11811, .F. ) ;
#2249 = VERTEX_POINT ( 'NONE', #5209 ) ;
#2250 = VERTEX_POINT ( 'NONE', #4431 ) ;
#2251 = CARTESIAN_POINT ( 'NONE',  ( 0.000000000000000000, 66.00000000000000000, -5.741599279633704455E-16 ) ) ;
#2252 = CARTESIAN_POINT ( 'NONE',  ( 10.00000000000000000, 376.0487089519831443, -75.00000000000331113 ) ) ;
#2253 = VECTOR ( 'NONE', #8755, 1000.000000000000000 ) ;
#2254 = EDGE_CURVE ( 'NONE', #11097, #1073, #9022, .T. ) ;
#2255 = FACE_OUTER_BOUND ( 'NONE', #2494, .T. ) ;
#2256 = LINE ( 'NONE', #4839, #12983 ) ;
#2257 = CARTESIAN_POINT ( 'NONE',  ( 1.750000000000000000, 14.59999999999999964, 0.000000000000000000 ) ) ;
#2258 = CARTESIAN_POINT ( 'NONE',  ( 55.99999999999989342, 493.2350855268092573, -580.5705369404290650 ) ) ;
#2259 = AXIS2_PLACEMENT_3D ( 'NONE', #8392, #11287, #11375 ) ;
#2260 = FACE_OUTER_BOUND ( 'NONE', #13023, .T. ) ;
#2261 = CIRCLE ( 'NONE', #8580, 4.695405383896011919 ) ;
#2262 = ADVANCED_FACE ( 'NONE', ( #7788 ), #5633, .F. ) ;
#2263 = ORIENTED_EDGE ( 'NONE', *, *, #12358, .F. ) ;
#2264 = LINE ( 'NONE', #16770, #16105 ) ;
#2265 = CARTESIAN_POINT ( 'NONE',  ( 31.00000000000000000, 19.00000000000000000, -21.00000000000000355 ) ) ;
#2266 = ORIENTED_EDGE ( 'NONE', *, *, #5198, .T. ) ;
#2267 = EDGE_CURVE ( 'NONE', #11960, #7984, #4354, .T. ) ;
#2268 = EDGE_CURVE ( 'NONE', #11320, #7813, #1276, .T. ) ;
#2269 = EDGE_CURVE ( 'NONE', #9495, #13726, #15598, .T. ) ;
#2270 = DIRECTION ( 'NONE',  ( 0.000000000000000000, 0.000000000000000000, -1.000000000000000000 ) ) ;
#2272 = ORIENTED_EDGE ( 'NONE', *, *, #1439, .T. ) ;
#2271 = ORIENTED_EDGE ( 'NONE', *, *, #12212, .F. ) ;
#2273 = CIRCLE ( 'NONE', #1456, 7.999999999999996447 ) ;
#2274 = DIRECTION ( 'NONE',  ( -3.854941057726253874E-16, 0.000000000000000000, -1.000000000000000000 ) ) ;
#2275 = DIRECTION ( 'NONE',  ( 0.000000000000000000, 0.000000000000000000, -1.000000000000000000 ) ) ;
#2276 = VECTOR ( 'NONE', #8935, 1000.000000000000000 ) ;
#2277 = CIRCLE ( 'NONE', #3929, 4.999999999999997335 ) ;
#2278 = DIRECTION ( 'NONE',  ( 0.000000000000000000, -6.028905917052134721E-13, 1.000000000000000000 ) ) ;
#2279 = CARTESIAN_POINT ( 'NONE',  ( 45.00000000000000000, 515.4878487013597805, -486.7230258972047636 ) ) ;
#2280 = ORIENTED_EDGE ( 'NONE', *, *, #10841, .T. ) ;
#2281 = UNCERTAINTY_MEASURE_WITH_UNIT (LENGTH_MEASURE( 1.000000000000000082E-05 ), #3261, 'distance_accuracy_value', 'NONE');
#2282 = CARTESIAN_POINT ( 'NONE',  ( 0.000000000000000000, 10.00000000000000000, -12.00000000000000178 ) ) ;
#2283 = CIRCLE ( 'NONE', #10250, 7.999999999999996447 ) ;
#2284 = CARTESIAN_POINT ( 'NONE',  ( -45.00000000000000000, 515.4878487013597805, -546.7230258972048205 ) ) ;
#2285 = ORIENTED_EDGE ( 'NONE', *, *, #13399, .F. ) ;
#2286 = PLANE ( 'NONE',  #13168 ) ;
#2287 = CARTESIAN_POINT ( 'NONE',  ( -2.220446049250313081E-13, 135.5000000000000000, 3.000000000000000000 ) ) ;
#2288 = DIRECTION ( 'NONE',  ( 0.000000000000000000, 0.000000000000000000, -1.000000000000000000 ) ) ;
#2289 = CIRCLE ( 'NONE', #107, 15.00000000000000000 ) ;
#2290 = CIRCLE ( 'NONE', #4227, 2.999999999999999112 ) ;
#2291 = EDGE_CURVE ( 'NONE', #1561, #16924, #16026, .T. ) ;
#2292 = CARTESIAN_POINT ( 'NONE',  ( 55.99999999999989342, 559.9933750504617365, -551.4184312811007658 ) ) ;
#2293 = CYLINDRICAL_SURFACE ( 'NONE', #12560, 13.69540538389601991 ) ;
#2294 = VERTEX_POINT ( 'NONE', #13459 ) ;
#2295 = CARTESIAN_POINT ( 'NONE',  ( -31.81980515339462912, 0.000000000000000000, -28.51980515339464972 ) ) ;
#2296 = AXIS2_PLACEMENT_3D ( 'NONE', #4671, #8207, #1781 ) ;
#2297 = DIRECTION ( 'NONE',  ( 0.000000000000000000, 1.000000000000000000, 0.000000000000000000 ) ) ;
#2298 = CIRCLE ( 'NONE', #16029, 4.695405383896011919 ) ;
#2299 = ORIENTED_EDGE ( 'NONE', *, *, #4684, .T. ) ;
#2300 = VECTOR ( 'NONE', #14206, 1000.000000000000000 ) ;
#2301 = VECTOR ( 'NONE', #16413, 1000.000000000000000 ) ;
#2302 = CARTESIAN_POINT ( 'NONE',  ( 3.674999999999999822, 0.000000000000000000, 0.000000000000000000 ) ) ;
#2303 = ADVANCED_FACE ( 'NONE', ( #10957 ), #12328, .F. ) ;
#2304 = DIRECTION ( 'NONE',  ( -1.000000000000000000, 0.000000000000000000, -0.000000000000000000 ) ) ;
#2305 = ORIENTED_EDGE ( 'NONE', *, *, #2246, .T. ) ;
#2306 = FACE_OUTER_BOUND ( 'NONE', #12787, .T. ) ;
#2307 = VECTOR ( 'NONE', #5057, 1000.000000000000000 ) ;
#2308 = CARTESIAN_POINT ( 'NONE',  ( 394.0000000000001137, 341.4647406485092915, -16.00114864346762644 ) ) ;
#2309 = DIRECTION ( 'NONE',  ( 1.000000000000000000, -0.000000000000000000, -0.000000000000000000 ) ) ;
#2310 = ORIENTED_EDGE ( 'NONE', *, *, #13715, .T. ) ;
#2311 = EDGE_CURVE ( 'NONE', #5700, #13853, #2884, .T. ) ;
#2312 = DIRECTION ( 'NONE',  ( 0.000000000000000000, 0.000000000000000000, -1.000000000000000000 ) ) ;
#2313 = CARTESIAN_POINT ( 'NONE',  ( 39.99999999999999289, 8.000000000000000000, 18.99999999999999645 ) ) ;
#2314 = ORIENTED_EDGE ( 'NONE', *, *, #1324, .F. ) ;
#2315 = CARTESIAN_POINT ( 'NONE',  ( 34.99999999999997868, 8.000000000000000000, -40.00000000000000711 ) ) ;
#2316 = AXIS2_PLACEMENT_3D ( 'NONE', #14453, #10329, #2676 ) ;
#2317 = VECTOR ( 'NONE', #5404, 1000.000000000000000 ) ;
#2318 = SHAPE_REPRESENTATION_RELATIONSHIP ( 'NONE' , 'NONE' ,  #25, #7495 ) ;
#2319 = AXIS2_PLACEMENT_3D ( 'NONE', #7354, #16390, #5740 ) ;
#2320 = EDGE_LOOP ( 'NONE', ( #4624, #13141 ) ) ;
#2321 = DIRECTION ( 'NONE',  ( 0.000000000000000000, -1.000000000000000000, 0.000000000000000000 ) ) ;
#2322 = LINE ( 'NONE', #5143, #5604 ) ;
#2323 = DIRECTION ( 'NONE',  ( 0.000000000000000000, 0.000000000000000000, -1.000000000000000000 ) ) ;
#2324 = ORIENTED_EDGE ( 'NONE', *, *, #6516, .T. ) ;
#2325 = CARTESIAN_POINT ( 'NONE',  ( 31.00000000000006395, 68.00000000000000000, -22.99999999999999289 ) ) ;
#2326 = LINE ( 'NONE', #11183, #11674 ) ;
#2327 = ORIENTED_EDGE ( 'NONE', *, *, #7806, .T. ) ;
#2328 = VECTOR ( 'NONE', #3317, 1000.000000000000000 ) ;
#2329 = DIRECTION ( 'NONE',  ( 0.000000000000000000, 0.000000000000000000, 1.000000000000000000 ) ) ;
#2330 = ORIENTED_EDGE ( 'NONE', *, *, #10754, .T. ) ;
#2331 = ORIENTED_EDGE ( 'NONE', *, *, #9144, .T. ) ;
#2332 = DIRECTION ( 'NONE',  ( 1.000000000000000000, 0.000000000000000000, 0.000000000000000000 ) ) ;
#2333 = ORIENTED_EDGE ( 'NONE', *, *, #5410, .F. ) ;
#2334 = DIRECTION ( 'NONE',  ( 1.000000000000000000, 0.000000000000000000, 0.000000000000000000 ) ) ;
#2335 = EDGE_CURVE ( 'NONE', #9156, #15233, #1882, .T. ) ;
#2336 = ORIENTED_EDGE ( 'NONE', *, *, #7070, .T. ) ;
#2337 = ORIENTED_EDGE ( 'NONE', *, *, #1652, .T. ) ;
#2338 = AXIS2_PLACEMENT_3D ( 'NONE', #10946, #8276, #16097 ) ;
#2339 = PLANE ( 'NONE',  #337 ) ;
#2340 = CARTESIAN_POINT ( 'NONE',  ( -23.00000000000002132, 10.00000000000000000, 31.00000000000003553 ) ) ;
#2341 = EDGE_CURVE ( 'NONE', #1150, #1698, #5719, .T. ) ;
#2342 = CARTESIAN_POINT ( 'NONE',  ( 10.00000000000000000, 309.2289037985890445, -146.8198051533984199 ) ) ;
#2343 = DIRECTION ( 'NONE',  ( 1.000000000000000000, 0.000000000000000000, -0.000000000000000000 ) ) ;
#2344 = FACE_OUTER_BOUND ( 'NONE', #873, .T. ) ;
#2345 = CARTESIAN_POINT ( 'NONE',  ( 394.0000000000001137, 451.4647406485094621, 28.44173619839933309 ) ) ;
#2346 = DIRECTION ( 'NONE',  ( -0.000000000000000000, -1.000000000000000000, -0.000000000000000000 ) ) ;
#2347 = ORIENTED_EDGE ( 'NONE', *, *, #8559, .T. ) ;
#2348 = FACE_OUTER_BOUND ( 'NONE', #7908, .T. ) ;
#2349 = CARTESIAN_POINT ( 'NONE',  ( 0.000000000000000000, 451.4647406485094621, 28.44173619839933309 ) ) ;
#2350 = ORIENTED_EDGE ( 'NONE', *, *, #10641, .F. ) ;
#2351 = AXIS2_PLACEMENT_3D ( 'NONE', #9806, #8505, #13745 ) ;
#2352 = AXIS2_PLACEMENT_3D ( 'NONE', #11797, #40, #2779 ) ;
#2353 = DIRECTION ( 'NONE',  ( -0.000000000000000000, -1.000000000000000000, -0.000000000000000000 ) ) ;
#2355 = ORIENTED_EDGE ( 'NONE', *, *, #9623, .T. ) ;
#2354 = VERTEX_POINT ( 'NONE', #8289 ) ;
#2356 = LINE ( 'NONE', #6131, #16867 ) ;
#2357 = ADVANCED_FACE ( 'NONE', ( #13631 ), #13545, .F. ) ;
#2358 = CARTESIAN_POINT ( 'NONE',  ( 17.99999999999998224, 10.00000000000000000, -36.99999999999999289 ) ) ;
#2359 = DIRECTION ( 'NONE',  ( -1.000000000000000000, -0.000000000000000000, -0.000000000000000000 ) ) ;
#2360 = EDGE_CURVE ( 'NONE', #6025, #4071, #4172, .T. ) ;
#2361 = CYLINDRICAL_SURFACE ( 'NONE', #1190, 22.75209553982836397 ) ;
#2362 = EDGE_CURVE ( 'NONE', #8007, #14343, #6818, .T. ) ;
#2363 = AXIS2_PLACEMENT_3D ( 'NONE', #6303, #2627, #15673 ) ;
#2365 = VERTEX_POINT ( 'NONE', #13783 ) ;
#2364 = EDGE_CURVE ( 'NONE', #16504, #10947, #6037, .T. ) ;
#2366 = VECTOR ( 'NONE', #7110, 1000.000000000000000 ) ;
#2367 = EDGE_CURVE ( 'NONE', #3583, #1386, #6527, .T. ) ;
#2368 = DIRECTION ( 'NONE',  ( 1.000000000000000000, 0.000000000000000000, 0.000000000000000000 ) ) ;
#2369 = VERTEX_POINT ( 'NONE', #4595 ) ;
#2370 = DIRECTION ( 'NONE',  ( 1.000000000000000000, 0.000000000000000000, 0.000000000000000000 ) ) ;
#2371 = APPLICATION_CONTEXT ( 'automotive_design' ) ;
#2372 = CARTESIAN_POINT ( 'NONE',  ( 45.00000000000000000, 515.4878487013597805, -546.7230258972048205 ) ) ;
#2373 = FACE_OUTER_BOUND ( 'NONE', #1913, .T. ) ;
#2374 = DIRECTION ( 'NONE',  ( -7.900838015626929923E-17, -8.586860021784410058E-33, 1.000000000000000000 ) ) ;
#2375 = DIRECTION ( 'NONE',  ( 1.000000000000000000, -0.000000000000000000, 0.000000000000000000 ) ) ;
#2376 = ORIENTED_EDGE ( 'NONE', *, *, #13793, .F. ) ;
#2377 = CIRCLE ( 'NONE', #1038, 13.69540538389601991 ) ;
#2378 = DIRECTION ( 'NONE',  ( 4.930380657631322689E-32, 0.09950371902099953980, 0.9950371902099890420 ) ) ;
#2379 = CIRCLE ( 'NONE', #1557, 14.59999999999999964 ) ;
#2380 = CARTESIAN_POINT ( 'NONE',  ( 45.00000000000000000, 549.5810598491749488, -589.0260321808809749 ) ) ;
#2381 = EDGE_CURVE ( 'NONE', #7827, #7102, #11205, .T. ) ;
#2382 = CARTESIAN_POINT ( 'NONE',  ( 5.687501635565830327, 12.64907335584850046, 0.000000000000000000 ) ) ;
#2383 = ADVANCED_FACE ( 'NONE', ( #2260 ), #16691, .T. ) ;
#2384 = ORIENTED_EDGE ( 'NONE', *, *, #12010, .T. ) ;
#2385 = EDGE_CURVE ( 'NONE', #3814, #4858, #820, .T. ) ;
#2386 = DIRECTION ( 'NONE',  ( 0.000000000000000000, 7.137148015447440312E-15, -1.000000000000000000 ) ) ;
#2387 = AXIS2_PLACEMENT_3D ( 'NONE', #14335, #7964, #14508 ) ;
#2388 = DIRECTION ( 'NONE',  ( 0.000000000000000000, 0.000000000000000000, 1.000000000000000000 ) ) ;
#2389 = EDGE_LOOP ( 'NONE', ( #9364, #5145, #10593, #15478 ) ) ;
#2390 = FACE_OUTER_BOUND ( 'NONE', #621, .T. ) ;
#2391 = LINE ( 'NONE', #7536, #14228 ) ;
#2392 = LINE ( 'NONE', #9186, #6737 ) ;
#2393 = ORIENTED_EDGE ( 'NONE', *, *, #16215, .F. ) ;
#2394 =( NAMED_UNIT ( * ) SI_UNIT ( $, .STERADIAN. ) SOLID_ANGLE_UNIT ( ) );
#2395 = DIRECTION ( 'NONE',  ( 1.000000000000000000, -0.000000000000000000, 0.000000000000000000 ) ) ;
#2396 = DIRECTION ( 'NONE',  ( 0.000000000000000000, -0.3746065934159049648, -0.9271838545667903109 ) ) ;
#2397 = ORIENTED_EDGE ( 'NONE', *, *, #6460, .T. ) ;
#2398 = EDGE_CURVE ( 'NONE', #4190, #15569, #15055, .T. ) ;
#2399 = VECTOR ( 'NONE', #6152, 1000.000000000000000 ) ;
#2400 = SHAPE_REPRESENTATION_RELATIONSHIP ( 'NONE' , 'NONE' ,  #8805, #10584 ) ;
#2401 = ORIENTED_EDGE ( 'NONE', *, *, #2476, .F. ) ;
#2402 = CARTESIAN_POINT ( 'NONE',  ( 22.99999999999999289, 68.00000000000000000, 37.00000000000002132 ) ) ;
#2403 = FACE_OUTER_BOUND ( 'NONE', #9739, .T. ) ;
#2404 = PLANE ( 'NONE',  #5201 ) ;
#2405 = ORIENTED_EDGE ( 'NONE', *, *, #1012, .T. ) ;
#2406 = DIRECTION ( 'NONE',  ( 1.000000000000000000, -0.000000000000000000, 0.000000000000000000 ) ) ;
#2407 = LINE ( 'NONE', #14266, #14703 ) ;
#2408 = ORIENTED_EDGE ( 'NONE', *, *, #4465, .T. ) ;
#2409 = AXIS2_PLACEMENT_3D ( 'NONE', #10571, #8076, #6513 ) ;
#2410 = CARTESIAN_POINT ( 'NONE',  ( 0.7366000000000293424, 218.4499468633031825, 287.1312267635914850 ) ) ;
#2411 = ORIENTED_EDGE ( 'NONE', *, *, #16716, .T. ) ;
#2412 = VERTEX_POINT ( 'NONE', #13957 ) ;
#2413 = LINE ( 'NONE', #16921, #14094 ) ;
#2414 = ORIENTED_EDGE ( 'NONE', *, *, #16539, .T. ) ;
#2415 = CARTESIAN_POINT ( 'NONE',  ( 446.7299999999998477, 475.6860672256533462, -37.52989836422094072 ) ) ;
#2416 = ORIENTED_EDGE ( 'NONE', *, *, #10060, .T. ) ;
#2417 = ORIENTED_EDGE ( 'NONE', *, *, #4995, .T. ) ;
#2418 = VECTOR ( 'NONE', #2970, 1000.000000000000000 ) ;
#2419 = SHAPE_REPRESENTATION ( 'Part4', ( #1488 ), #15488 ) ;
#2420 = DIRECTION ( 'NONE',  ( -0.000000000000000000, -1.000000000000000000, -0.000000000000000000 ) ) ;
#2421 = CARTESIAN_POINT ( 'NONE',  ( 10.00000000000000000, 620.7506394335853201, -11.00000000000000000 ) ) ;
#2422 = ORIENTED_EDGE ( 'NONE', *, *, #1627, .T. ) ;
#2423 = CARTESIAN_POINT ( 'NONE',  ( 5.950000000000000178, -12.65000000000000036, -1.701720561796546765E-15 ) ) ;
#2424 = PLANE ( 'NONE',  #5028 ) ;
#2425 = EDGE_CURVE ( 'NONE', #4130, #7948, #11284, .T. ) ;
#2426 = DIRECTION ( 'NONE',  ( -0.000000000000000000, -1.000000000000000000, -0.000000000000000000 ) ) ;
#2427 = DIRECTION ( 'NONE',  ( -1.000000000000000000, 0.000000000000000000, 0.000000000000000000 ) ) ;
#2428 = EDGE_LOOP ( 'NONE', ( #9790, #15179, #726, #9313 ) ) ;
#2429 = CARTESIAN_POINT ( 'NONE',  ( 0.000000000000000000, 451.4647406485092915, -149.8062676851188257 ) ) ;
#2430 = CARTESIAN_POINT ( 'NONE',  ( 0.000000000000000000, 339.3157724647196005, -16.41886574335978821 ) ) ;
#2431 = EDGE_LOOP ( 'NONE', ( #6016, #12758 ) ) ;
#2432 = LINE ( 'NONE', #5010, #10989 ) ;
#2433 = ORIENTED_EDGE ( 'NONE', *, *, #5335, .F. ) ;
#2434 = EDGE_CURVE ( 'NONE', #1511, #2958, #5881, .T. ) ;
#2435 = DIRECTION ( 'NONE',  ( 0.000000000000000000, 0.000000000000000000, 1.000000000000000000 ) ) ;
#2436 = ORIENTED_EDGE ( 'NONE', *, *, #4789, .F. ) ;
#2437 = AXIS2_PLACEMENT_3D ( 'NONE', #13629, #11123, #6036 ) ;
#2438 = ORIENTED_EDGE ( 'NONE', *, *, #13739, .F. ) ;
#2439 = PLANE ( 'NONE',  #6907 ) ;
#2440 = FACE_OUTER_BOUND ( 'NONE', #11887, .T. ) ;
#2441 = PLANE ( 'NONE',  #12971 ) ;
#2442 = VERTEX_POINT ( 'NONE', #8542 ) ;
#2443 = PRODUCT ( 'din_6885_2_a_6_x_6_x_25', 'din_6885_2_a_6_x_6_x_25', '', ( #11008 ) ) ;
#2444 = DIRECTION ( 'NONE',  ( 0.000000000000000000, 0.000000000000000000, -1.000000000000000000 ) ) ;
#2445 = EDGE_CURVE ( 'NONE', #6153, #2950, #1673, .T. ) ;
#2446 = LINE ( 'NONE', #15670, #6850 ) ;
#2447 = ADVANCED_FACE ( 'NONE', ( #4752, #10009, #12659, #984, #2179, #741, #5963, #6203, #13870, #4518, #8800 ), #10091, .T. ) ;
#2448 = DIRECTION ( 'NONE',  ( -1.000000000000000000, -0.000000000000000000, -0.000000000000000000 ) ) ;
#2449 = FACE_OUTER_BOUND ( 'NONE', #10149, .T. ) ;
#2450 = AXIS2_PLACEMENT_3D ( 'NONE', #15022, #11233, #16643 ) ;
#2451 = DIRECTION ( 'NONE',  ( -1.000000000000000000, -0.000000000000000000, -0.000000000000000000 ) ) ;
#2452 = LINE ( 'NONE', #6478, #12608 ) ;
#2454 = VERTEX_POINT ( 'NONE', #8723 ) ;
#2453 = EDGE_LOOP ( 'NONE', ( #1841, #7875, #9989, #13838, #8877 ) ) ;
#2455 = EDGE_CURVE ( 'NONE', #1693, #3926, #7491, .T. ) ;
#2456 = ADVANCED_FACE ( 'NONE', ( #901 ), #7150, .F. ) ;
#2457 = EDGE_CURVE ( 'NONE', #14614, #16035, #3395, .T. ) ;
#2458 = CARTESIAN_POINT ( 'NONE',  ( -40.00000000000000711, 10.00000000000000000, 26.00000000000000000 ) ) ;
#2459 = ADVANCED_FACE ( 'NONE', ( #16610 ), #15327, .F. ) ;
#2460 = DIRECTION ( 'NONE',  ( -1.000000000000000000, -0.000000000000000000, -1.156482317317870344E-15 ) ) ;
#2461 = DIRECTION ( 'NONE',  ( -1.000000000000000000, 0.000000000000000000, 0.000000000000000000 ) ) ;
#2462 = STYLED_ITEM ( 'NONE', ( #5720 ), #8939 ) ;
#2463 = ORIENTED_EDGE ( 'NONE', *, *, #8025, .F. ) ;
#2464 = CIRCLE ( 'NONE', #6029, 13.69540538389596485 ) ;
#2465 = DIRECTION ( 'NONE',  ( 0.000000000000000000, 0.000000000000000000, 1.000000000000000000 ) ) ;
#2466 = CARTESIAN_POINT ( 'NONE',  ( 34.99999999999997868, 11.00000000000000000, -40.00000000000000711 ) ) ;
#2467 = ORIENTED_EDGE ( 'NONE', *, *, #2534, .F. ) ;
#2468 = LINE ( 'NONE', #3689, #13835 ) ;
#2469 = CARTESIAN_POINT ( 'NONE',  ( 4.025000000000000355, -17.52499999999999858, -2.146193515505736390E-15 ) ) ;
#2470 = CARTESIAN_POINT ( 'NONE',  ( 0.000000000000000000, 481.5601199098531993, -512.1772732904406666 ) ) ;
#2471 = ORIENTED_EDGE ( 'NONE', *, *, #16722, .F. ) ;
#2472 = CARTESIAN_POINT ( 'NONE',  ( 1.750000000000000000, 0.000000000000000000, 0.000000000000000000 ) ) ;
#2473 = CARTESIAN_POINT ( 'NONE',  ( 0.000000000000000000, 226.8713558223388134, -346.2582248962859808 ) ) ;
#2474 = CARTESIAN_POINT ( 'NONE',  ( 0.07938566280166349520, 285.8325239394490609, 37.43526655022222371 ) ) ;
#2475 = ORIENTED_EDGE ( 'NONE', *, *, #1932, .F. ) ;
#2476 = EDGE_CURVE ( 'NONE', #12820, #14037, #6620, .T. ) ;
#2477 = EDGE_CURVE ( 'NONE', #12375, #16649, #92, .T. ) ;
#2478 = AXIS2_PLACEMENT_3D ( 'NONE', #14214, #11539, #6285 ) ;
#2479 = CARTESIAN_POINT ( 'NONE',  ( 0.000000000000000000, 301.0487089519832011, -80.00000000000387956 ) ) ;
#2480 = EDGE_CURVE ( 'NONE', #14915, #3142, #7208, .T. ) ;
#2481 = CARTESIAN_POINT ( 'NONE',  ( 30.90550859392671157, 32.88608451763352747, 66.87703344121199223 ) ) ;
#2482 = DIRECTION ( 'NONE',  ( 0.000000000000000000, 0.000000000000000000, -1.000000000000000000 ) ) ;
#2483 = EDGE_LOOP ( 'NONE', ( #9993, #4850 ) ) ;
#2484 = DIRECTION ( 'NONE',  ( 1.000000000000000000, 0.000000000000000000, 0.000000000000000000 ) ) ;
#2485 = DIRECTION ( 'NONE',  ( 0.000000000000000000, 0.000000000000000000, -1.000000000000000000 ) ) ;
#2486 = AXIS2_PLACEMENT_3D ( 'NONE', #13123, #1528, #9259 ) ;
#2487 = CARTESIAN_POINT ( 'NONE',  ( -26.00000000000000000, 11.00000000000000000, 40.00000000000000711 ) ) ;
#2488 = ORIENTED_EDGE ( 'NONE', *, *, #14023, .F. ) ;
#2489 = DIRECTION ( 'NONE',  ( 1.000000000000000000, 0.000000000000000000, 0.000000000000000000 ) ) ;
#2490 = DIRECTION ( 'NONE',  ( -0.000000000000000000, 1.000000000000000000, -0.000000000000000000 ) ) ;
#2491 = ORIENTED_EDGE ( 'NONE', *, *, #5705, .T. ) ;
#2492 = DIRECTION ( 'NONE',  ( -1.000000000000000000, 0.000000000000000000, 0.000000000000000000 ) ) ;
#2493 = VERTEX_POINT ( 'NONE', #31 ) ;
#2494 = EDGE_LOOP ( 'NONE', ( #16571, #5730, #15677, #9076 ) ) ;
#2495 = DIRECTION ( 'NONE',  ( 0.000000000000000000, 0.000000000000000000, -1.000000000000000000 ) ) ;
#2496 = EDGE_LOOP ( 'NONE', ( #2651, #12373, #14289, #8279 ) ) ;
#2497 = DIRECTION ( 'NONE',  ( 0.000000000000000000, 0.000000000000000000, 1.000000000000000000 ) ) ;
#2498 = AXIS2_PLACEMENT_3D ( 'NONE', #10868, #1594, #7067 ) ;
#2499 = EDGE_LOOP ( 'NONE', ( #2690, #11700, #7081 ) ) ;
#2500 = ORIENTED_EDGE ( 'NONE', *, *, #13369, .T. ) ;
#2501 = VECTOR ( 'NONE', #1362, 1000.000000000000000 ) ;
#2502 = CLOSED_SHELL ( 'NONE', ( #16619, #10825, #12339, #15141, #3509, #1728, #12688, #5427, #9181, #962, #671, #14093, #2459, #4372, #6873, #6526, #12645, #5405, #2900, #992, #1388, #9202, #9818, #9654, #13487, #12666, #10827, #15913, #16741, #10107, #12050, #4042, #12928, #6762 ) ) ;
#2503 = CARTESIAN_POINT ( 'NONE',  ( -3.270000000000000462, 258.7934930265974458, 287.5298983642207986 ) ) ;
#2504 = LINE ( 'NONE', #1058, #661 ) ;
#2505 = ORIENTED_EDGE ( 'NONE', *, *, #5403, .T. ) ;
#2506 = CARTESIAN_POINT ( 'NONE',  ( 31.81980515339464333, 11.00000000000000000, 28.51980515339463906 ) ) ;
#2507 = CARTESIAN_POINT ( 'NONE',  ( -31.00000000000003553, 19.00000000000000000, 25.99999999999999645 ) ) ;
#2508 = AXIS2_PLACEMENT_3D ( 'NONE', #8631, #11119, #9835 ) ;
#2509 = DIRECTION ( 'NONE',  ( 0.000000000000000000, 0.8660254037844432595, -0.4999999999999919509 ) ) ;
#2510 = ORIENTED_EDGE ( 'NONE', *, *, #1039, .T. ) ;
#2511 = CARTESIAN_POINT ( 'NONE',  ( 0.000000000000000000, 364.9870314427752191, -206.3519347178565795 ) ) ;
#2512 = PLANE ( 'NONE',  #8316 ) ;
#2513 = ORIENTED_EDGE ( 'NONE', *, *, #14679, .F. ) ;
#2514 = AXIS2_PLACEMENT_3D ( 'NONE', #12437, #3422, #14939 ) ;
#2515 = AXIS2_PLACEMENT_3D ( 'NONE', #2624, #15594, #7852 ) ;
#2516 = EDGE_CURVE ( 'NONE', #15471, #3705, #6279, .T. ) ;
#2517 = CIRCLE ( 'NONE', #11026, 2.500000000000002220 ) ;
#2518 = AXIS2_PLACEMENT_3D ( 'NONE', #4012, #2288, #15430 ) ;
#2519 = AXIS2_PLACEMENT_3D ( 'NONE', #16622, #11464, #10357 ) ;
#2520 = CARTESIAN_POINT ( 'NONE',  ( -40.00000000000000000, 68.00000000000000000, 26.00000000000000355 ) ) ;
#2521 = VERTEX_POINT ( 'NONE', #14285 ) ;
#2522 = PLANE ( 'NONE',  #9479 ) ;
#2523 = VERTEX_POINT ( 'NONE', #1400 ) ;
#2524 = AXIS2_PLACEMENT_3D ( 'NONE', #6774, #9624, #15878 ) ;
#2525 = ORIENTED_EDGE ( 'NONE', *, *, #4192, .T. ) ;
#2526 = FACE_BOUND ( 'NONE', #12867, .T. ) ;
#2527 = PRODUCT_RELATED_PRODUCT_CATEGORY ( 'part', '', ( #2165 ) ) ;
#2528 = FACE_OUTER_BOUND ( 'NONE', #611, .T. ) ;
#2529 = LINE ( 'NONE', #9155, #8040 ) ;
#2530 = ORIENTED_EDGE ( 'NONE', *, *, #13582, .F. ) ;
#2531 = LINE ( 'NONE', #9407, #7166 ) ;
#2532 = VECTOR ( 'NONE', #13906, 1000.000000000000000 ) ;
#2533 = CARTESIAN_POINT ( 'NONE',  ( 4.899999999999999467, 12.00000000000000000, 0.000000000000000000 ) ) ;
#2534 = EDGE_CURVE ( 'NONE', #6207, #5894, #2830, .T. ) ;
#2535 = DIRECTION ( 'NONE',  ( 0.000000000000000000, 0.7071067811865445751, 0.7071067811865504593 ) ) ;
#2536 = CARTESIAN_POINT ( 'NONE',  ( -40.00000000000000000, 0.000000000000000000, -25.99999999999999645 ) ) ;
#2537 = CARTESIAN_POINT ( 'NONE',  ( 39.99999999999999289, 10.00000000000000000, 26.00000000000000000 ) ) ;
#2538 = AXIS2_PLACEMENT_3D ( 'NONE', #9525, #13475, #6832 ) ;
#2539 = CARTESIAN_POINT ( 'NONE',  ( -150.0000000000000284, 620.7506394335853201, 0.000000000000000000 ) ) ;
#2540 = DIRECTION ( 'NONE',  ( 0.000000000000000000, 1.000000000000000000, 0.000000000000000000 ) ) ;
#2542 = ORIENTED_EDGE ( 'NONE', *, *, #14861, .F. ) ;
#2541 = ORIENTED_EDGE ( 'NONE', *, *, #11717, .F. ) ;
#2543 = DIRECTION ( 'NONE',  ( 1.000000000000000000, -0.000000000000000000, 0.000000000000000000 ) ) ;
#2544 = VECTOR ( 'NONE', #10813, 1000.000000000000000 ) ;
#2545 = CIRCLE ( 'NONE', #366, 18.46360580700775245 ) ;
#2546 = CIRCLE ( 'NONE', #12162, 4.695405383896011919 ) ;
#2547 = CARTESIAN_POINT ( 'NONE',  ( 55.99999999999989342, 493.2350855268092573, -585.2659423243250103 ) ) ;
#2548 = EDGE_CURVE ( 'NONE', #10447, #4210, #16858, .T. ) ;
#2549 = PLANE ( 'NONE',  #6585 ) ;
#2550 = CARTESIAN_POINT ( 'NONE',  ( -25.99999999999999645, 68.00000000000000000, 31.00000000000003908 ) ) ;
#2551 = VECTOR ( 'NONE', #4412, 1000.000000000000000 ) ;
#2552 = ORIENTED_EDGE ( 'NONE', *, *, #6044, .T. ) ;
#2553 = CARTESIAN_POINT ( 'NONE',  ( 9.796850830579020038E-16, 6.000000000000000000, 22.00000000000000000 ) ) ;
#2554 = CIRCLE ( 'NONE', #12174, 13.69540538389601636 ) ;
#2555 = EDGE_CURVE ( 'NONE', #5137, #1233, #14629, .T. ) ;
#2556 = CIRCLE ( 'NONE', #8051, 17.52499999999999858 ) ;
#2557 = CARTESIAN_POINT ( 'NONE',  ( -1.776356839400249676E-15, 13.94999999999999929, 0.000000000000000000 ) ) ;
#2558 = ORIENTED_EDGE ( 'NONE', *, *, #2234, .T. ) ;
#2559 = DIRECTION ( 'NONE',  ( 0.000000000000000000, 0.000000000000000000, -1.000000000000000000 ) ) ;
#2560 = CIRCLE ( 'NONE', #11896, 8.000000000000000000 ) ;
#2561 = LINE ( 'NONE', #9090, #16417 ) ;
#2562 = DIRECTION ( 'NONE',  ( -0.000000000000000000, -0.000000000000000000, 1.000000000000000000 ) ) ;
#2563 = VERTEX_POINT ( 'NONE', #3810 ) ;
#2564 = FILL_AREA_STYLE ('',( #16899 ) ) ;
#2565 = LINE ( 'NONE', #16814, #16386 ) ;
#2566 = CARTESIAN_POINT ( 'NONE',  ( -36.99999999999997868, 3.000000000000000000, -19.99999999999999289 ) ) ;
#2567 = EDGE_LOOP ( 'NONE', ( #12635, #7568, #4570, #4892 ) ) ;
#2568 = AXIS2_PLACEMENT_3D ( 'NONE', #16342, #16495, #7219 ) ;
#2569 = DIRECTION ( 'NONE',  ( 0.000000000000000000, 0.000000000000000000, 1.000000000000000000 ) ) ;
#2570 = CONTEXT_DEPENDENT_SHAPE_REPRESENTATION ( #2825, #5907 ) ;
#2571 = STYLED_ITEM ( 'NONE', ( #2161 ), #2894 ) ;
#2572 = AXIS2_PLACEMENT_3D ( 'NONE', #10859, #5701, #11025 ) ;
#2573 = DIRECTION ( 'NONE',  ( -6.982962677686266711E-15, 0.000000000000000000, -1.000000000000000000 ) ) ;
#2574 = EDGE_CURVE ( 'NONE', #11116, #793, #10418, .T. ) ;
#2575 = PLANE ( 'NONE',  #343 ) ;
#2576 = ORIENTED_EDGE ( 'NONE', *, *, #9804, .T. ) ;
#2577 = DIRECTION ( 'NONE',  ( -5.782411586589400040E-16, 0.000000000000000000, 1.000000000000000000 ) ) ;
#2578 = ADVANCED_FACE ( 'NONE', ( #4920 ), #15498, .T. ) ;
#2579 = CARTESIAN_POINT ( 'NONE',  ( 25.99999999999999645, 0.000000000000000000, 31.00000000000004619 ) ) ;
#2580 = AXIS2_PLACEMENT_3D ( 'NONE', #16476, #2055, #13992 ) ;
#2581 = ADVANCED_FACE ( 'NONE', ( #15406 ), #5166, .T. ) ;
#2582 = ADVANCED_FACE ( 'NONE', ( #6449, #10504 ), #14467, .T. ) ;
#2583 = DIRECTION ( 'NONE',  ( -0.000000000000000000, -0.000000000000000000, 1.000000000000000000 ) ) ;
#2584 = ORIENTED_EDGE ( 'NONE', *, *, #6022, .F. ) ;
#2585 = DIRECTION ( 'NONE',  ( 0.000000000000000000, 0.000000000000000000, 1.000000000000000000 ) ) ;
#2586 = ADVANCED_FACE ( 'NONE', ( #9138 ), #8888, .T. ) ;
#2587 = DIRECTION ( 'NONE',  ( -6.123031769111888756E-17, 1.000000000000000000, 3.749151804555344967E-33 ) ) ;
#2588 = VERTEX_POINT ( 'NONE', #1316 ) ;
#2589 = AXIS2_PLACEMENT_3D ( 'NONE', #15984, #6962, #1479 ) ;
#2590 = DIRECTION ( 'NONE',  ( 0.000000000000000000, 1.000000000000000000, -1.224646799147353207E-16 ) ) ;
#2591 = VECTOR ( 'NONE', #6590, 1000.000000000000000 ) ;
#2592 = ORIENTED_EDGE ( 'NONE', *, *, #8046, .F. ) ;
#2593 = ORIENTED_EDGE ( 'NONE', *, *, #2675, .T. ) ;
#2594 = CARTESIAN_POINT ( 'NONE',  ( 10.00000000000000000, 425.7506394335853201, 0.000000000000000000 ) ) ;
#2595 = AXIS2_PLACEMENT_3D ( 'NONE', #11249, #1896, #8434 ) ;
#2596 = ORIENTED_EDGE ( 'NONE', *, *, #10454, .F. ) ;
#2597 = B_SPLINE_SURFACE_WITH_KNOTS ( 'NONE', 1, 3, ( 
 ( #925, #12432, #7097, #3419, #16632, #9699, #15016, #13650, #4690, #8410 ),
 ( #8743, #9947, #8488, #7427, #677, #12350, #13893, #13729, #13976, #6148 ),
 ( #14935, #3174, #9786, #16384, #1950, #5905, #6060, #4614, #2117, #7348 ),
 ( #9862, #8914, #6386, #4865, #15599, #6225, #12777, #1169, #3919, #10288 ) ),
 .UNSPECIFIED., .F., .F., .F.,
 ( 2, 1, 1, 2 ),
 ( 4, 2, 2, 2, 4 ),
 ( -0.01000000000000000021, 0.000000000000000000, 1.000000000000000000, 1.010099999999999998 ),
 ( 0.000000000000000000, 0.2500000000000000000, 0.5000000000000000000, 0.7500000000000000000, 1.000000000000000000 ),
 .UNSPECIFIED. ) ;
#2598 = ORIENTED_EDGE ( 'NONE', *, *, #8043, .T. ) ;
#2599 = ORIENTED_EDGE ( 'NONE', *, *, #2080, .F. ) ;
#2600 = VERTEX_POINT ( 'NONE', #1144 ) ;
#2601 = LINE ( 'NONE', #3727, #14590 ) ;
#2602 = DIRECTION ( 'NONE',  ( -1.000000000000000000, -0.000000000000000000, -0.000000000000000000 ) ) ;
#2603 = VERTEX_POINT ( 'NONE', #1063 ) ;
#2604 = CIRCLE ( 'NONE', #7252, 13.69540538389601991 ) ;
#2605 = DIRECTION ( 'NONE',  ( 0.000000000000000000, 0.3853514969300962378, 0.9227698650333863162 ) ) ;
#2606 = EDGE_CURVE ( 'NONE', #7927, #9826, #14377, .T. ) ;
#2607 = CARTESIAN_POINT ( 'NONE',  ( 1.347066989204613998E-15, 0.000000000000000000, 22.00000000000000000 ) ) ;
#2608 = CYLINDRICAL_SURFACE ( 'NONE', #10612, 3.000000000000002665 ) ;
#2609 = CARTESIAN_POINT ( 'NONE',  ( 54.99999999999999289, 515.4878487013597805, -546.7230258972048205 ) ) ;
#2610 = ORIENTED_EDGE ( 'NONE', *, *, #1301, .T. ) ;
#2611 = LINE ( 'NONE', #7837, #7043 ) ;
#2612 = CARTESIAN_POINT ( 'NONE',  ( 0.000000000000000000, 451.4647406485092915, -149.8062676851188257 ) ) ;
#2613 = VERTEX_POINT ( 'NONE', #7835 ) ;
#2614 = DIRECTION ( 'NONE',  ( -1.000000000000000000, 0.000000000000000000, -0.000000000000000000 ) ) ;
#2615 = ORIENTED_EDGE ( 'NONE', *, *, #11497, .T. ) ;
#2616 = FACE_OUTER_BOUND ( 'NONE', #11012, .T. ) ;
#2617 = AXIS2_PLACEMENT_3D ( 'NONE', #9170, #12175, #12002 ) ;
#2618 = ORIENTED_EDGE ( 'NONE', *, *, #9274, .T. ) ;
#2619 = ORIENTED_EDGE ( 'NONE', *, *, #14017, .F. ) ;
#2620 = FACE_OUTER_BOUND ( 'NONE', #10894, .T. ) ;
#2621 = CARTESIAN_POINT ( 'NONE',  ( 25.99999999999999645, 68.00000000000000000, 31.00000000000004619 ) ) ;
#2622 = CARTESIAN_POINT ( 'NONE',  ( 31.00000000000006395, 0.000000000000000000, -22.99999999999999289 ) ) ;
#2623 = ORIENTED_EDGE ( 'NONE', *, *, #42, .F. ) ;
#2624 = CARTESIAN_POINT ( 'NONE',  ( 4.899999999999999467, 0.000000000000000000, 0.000000000000000000 ) ) ;
#2625 = DIRECTION ( 'NONE',  ( 0.000000000000000000, 0.000000000000000000, 1.000000000000000000 ) ) ;
#2626 = DIRECTION ( 'NONE',  ( 1.000000000000000000, 0.000000000000000000, 0.000000000000000000 ) ) ;
#2627 = DIRECTION ( 'NONE',  ( 0.000000000000000000, -1.000000000000000000, 0.000000000000000000 ) ) ;
#2628 = CARTESIAN_POINT ( 'NONE',  ( 10.00000000000000000, 620.7506394335853201, 109.9999999999999858 ) ) ;
#2629 = DIRECTION ( 'NONE',  ( -1.000000000000000000, -2.911324084205185756E-15, -2.422066625794664503E-16 ) ) ;
#2630 = DIRECTION ( 'NONE',  ( 0.000000000000000000, 0.000000000000000000, -1.000000000000000000 ) ) ;
#2632 = ORIENTED_EDGE ( 'NONE', *, *, #289, .F. ) ;
#2631 = ORIENTED_EDGE ( 'NONE', *, *, #170, .T. ) ;
#2633 = CARTESIAN_POINT ( 'NONE',  ( -31.00000000000003197, 68.00000000000000000, 26.00000000000000355 ) ) ;
#2634 = VECTOR ( 'NONE', #2562, 1000.000000000000000 ) ;
#2635 = FACE_BOUND ( 'NONE', #3168, .T. ) ;
#2636 = CARTESIAN_POINT ( 'NONE',  ( 31.00000000000006750, 19.00000000000000000, -21.00000000000000355 ) ) ;
#2637 = CARTESIAN_POINT ( 'NONE',  ( -22.00000000000001776, 6.000000000000000000, 32.00000000000000711 ) ) ;
#2638 = ORIENTED_EDGE ( 'NONE', *, *, #4767, .F. ) ;
#2639 = DIRECTION ( 'NONE',  ( 1.000000000000000000, 0.000000000000000000, 0.000000000000000000 ) ) ;
#2640 = DIRECTION ( 'NONE',  ( 0.000000000000000000, 0.000000000000000000, 1.000000000000000000 ) ) ;
#2641 = ORIENTED_EDGE ( 'NONE', *, *, #16745, .T. ) ;
#2642 = DIRECTION ( 'NONE',  ( 3.407805566942604354E-15, 0.9950371902099891530, -0.09950371902099955368 ) ) ;
#2643 = CARTESIAN_POINT ( 'NONE',  ( 10.00000000000000000, 620.7506394335853201, -11.00000000000000000 ) ) ;
#2644 = ORIENTED_EDGE ( 'NONE', *, *, #2867, .F. ) ;
#2645 = AXIS2_PLACEMENT_3D ( 'NONE', #11227, #15181, #15093 ) ;
#2646 = EDGE_CURVE ( 'NONE', #1389, #687, #13092, .T. ) ;
#2647 = AXIS2_PLACEMENT_3D ( 'NONE', #7015, #5812, #13803 ) ;
#2648 = DIRECTION ( 'NONE',  ( -0.000000000000000000, -1.000000000000000000, -0.000000000000000000 ) ) ;
#2649 = CARTESIAN_POINT ( 'NONE',  ( 10.00000000000000000, 34.88079231221936283, 28.80067286797032722 ) ) ;
#2650 = DIRECTION ( 'NONE',  ( 0.000000000000000000, 0.000000000000000000, -1.000000000000000000 ) ) ;
#2651 = ORIENTED_EDGE ( 'NONE', *, *, #8048, .F. ) ;
#2652 = CARTESIAN_POINT ( 'NONE',  ( -55.99999999999988631, 515.4878487013597805, -546.7230258972048205 ) ) ;
#2653 = ITEM_DEFINED_TRANSFORMATION ( 'NONE', 'NONE', #5040,  #1488 ) ;
#2654 = ADVANCED_FACE ( 'NONE', ( #6537 ), #6929, .T. ) ;
#2655 =( NAMED_UNIT ( * ) PLANE_ANGLE_UNIT ( ) SI_UNIT ( $, .RADIAN. ) );
#2656 = DIRECTION ( 'NONE',  ( -1.000000000000000000, 0.000000000000000000, -0.000000000000000000 ) ) ;
#2657 = VECTOR ( 'NONE', #12498, 1000.000000000000000 ) ;
#2658 = EDGE_LOOP ( 'NONE', ( #682, #2638 ) ) ;
#2659 = CARTESIAN_POINT ( 'NONE',  ( -30.99999999999999645, 0.000000000000000000, -30.99999999999999289 ) ) ;
#2660 = CARTESIAN_POINT ( 'NONE',  ( -19.00000000000001776, 8.000000000000000000, 36.00000000000000711 ) ) ;
#2661 = FACE_BOUND ( 'NONE', #9856, .T. ) ;
#2662 = VERTEX_POINT ( 'NONE', #380 ) ;
#2663 = CYLINDRICAL_SURFACE ( 'NONE', #5586, 29.99999999999530687 ) ;
#2664 = DIRECTION ( 'NONE',  ( -1.000000000000000000, -0.000000000000000000, -1.631319816340925608E-17 ) ) ;
#2665 = DIRECTION ( 'NONE',  ( 0.000000000000000000, 0.000000000000000000, 1.000000000000000000 ) ) ;
#2666 = ORIENTED_EDGE ( 'NONE', *, *, #11273, .F. ) ;
#2667 = EDGE_CURVE ( 'NONE', #1418, #15054, #8367, .T. ) ;
#2668 = CARTESIAN_POINT ( 'NONE',  ( 394.0000000000001137, 451.4647406485092915, -149.8062676851188257 ) ) ;
#2669 = EDGE_LOOP ( 'NONE', ( #6409, #15053, #13431, #10159 ) ) ;
#2670 = ORIENTED_EDGE ( 'NONE', *, *, #8487, .F. ) ;
#2671 = VECTOR ( 'NONE', #1034, 1000.000000000000000 ) ;
#2672 = DIRECTION ( 'NONE',  ( 0.000000000000000000, 0.000000000000000000, -1.000000000000000000 ) ) ;
#2673 = ORIENTED_EDGE ( 'NONE', *, *, #2242, .F. ) ;
#2674 = ORIENTED_EDGE ( 'NONE', *, *, #4848, .F. ) ;
#2675 = EDGE_CURVE ( 'NONE', #1629, #8468, #8037, .T. ) ;
#2676 = DIRECTION ( 'NONE',  ( 1.000000000000000000, 0.000000000000000000, 0.000000000000000000 ) ) ;
#2677 = EDGE_CURVE ( 'NONE', #12299, #1082, #213, .T. ) ;
#2678 = ADVANCED_FACE ( 'NONE', ( #13353 ), #4245, .T. ) ;
#2679 = EDGE_LOOP ( 'NONE', ( #11434, #1470, #16171, #11259 ) ) ;
#2680 = ORIENTED_EDGE ( 'NONE', *, *, #12164, .T. ) ;
#2681 = CARTESIAN_POINT ( 'NONE',  ( 3.000000000000000000, 1.836909530733565148E-16, 22.00000000000000000 ) ) ;
#2682 = DIRECTION ( 'NONE',  ( -0.000000000000000000, -1.000000000000000000, -0.000000000000000000 ) ) ;
#2683 = COLOUR_RGB ( '', 0.40784314, 0.44705882, 0.49803922) ;
#2684 = ORIENTED_EDGE ( 'NONE', *, *, #6535, .T. ) ;
#2685 = CARTESIAN_POINT ( 'NONE',  ( 46.99999999999988631, 473.6663340069158039, -548.2494070140132862 ) ) ;
#2686 = VECTOR ( 'NONE', #13454, 1000.000000000000000 ) ;
#2687 = CARTESIAN_POINT ( 'NONE',  ( -45.00000000000000000, 523.2161522479888163, -516.5890438806160319 ) ) ;
#2688 = ORIENTED_EDGE ( 'NONE', *, *, #14777, .F. ) ;
#2689 = DIRECTION ( 'NONE',  ( 0.000000000000000000, 0.000000000000000000, -1.000000000000000000 ) ) ;
#2690 = ORIENTED_EDGE ( 'NONE', *, *, #12030, .F. ) ;
#2691 = DIRECTION ( 'NONE',  ( 0.000000000000000000, 0.000000000000000000, 1.000000000000000000 ) ) ;
#2692 = CARTESIAN_POINT ( 'NONE',  ( 25.99999999999996092, 3.000000000000000000, 40.00000000000000711 ) ) ;
#2693 = ORIENTED_EDGE ( 'NONE', *, *, #15802, .F. ) ;
#2694 = DIRECTION ( 'NONE',  ( 0.000000000000000000, 0.000000000000000000, 1.000000000000000000 ) ) ;
#2695 = ORIENTED_EDGE ( 'NONE', *, *, #15747, .T. ) ;
#2696 = EDGE_CURVE ( 'NONE', #12703, #9577, #3660, .T. ) ;
#2697 = EDGE_CURVE ( 'NONE', #11977, #14614, #296, .T. ) ;
#2698 = LINE ( 'NONE', #3904, #718 ) ;
#2699 = ADVANCED_FACE ( 'NONE', ( #4415 ), #1838, .F. ) ;
#2700 = VECTOR ( 'NONE', #5132, 1000.000000000000000 ) ;
#2701 = EDGE_LOOP ( 'NONE', ( #6610, #10015, #12334, #1127, #15492, #13850 ) ) ;
#2702 = APPLICATION_CONTEXT ( 'automotive_design' ) ;
#2703 = ORIENTED_EDGE ( 'NONE', *, *, #2062, .T. ) ;
#2704 = FILL_AREA_STYLE ('',( #44 ) ) ;
#2705 = DIRECTION ( 'NONE',  ( 0.000000000000000000, 0.000000000000000000, -1.000000000000000000 ) ) ;
#2706 = DIRECTION ( 'NONE',  ( 0.000000000000000000, 0.000000000000000000, 1.000000000000000000 ) ) ;
#2707 = VERTEX_POINT ( 'NONE', #10677 ) ;
#2708 = LINE ( 'NONE', #7936, #12132 ) ;
#2709 = DIRECTION ( 'NONE',  ( 0.000000000000000000, 1.000000000000000000, 0.000000000000000000 ) ) ;
#2710 = CARTESIAN_POINT ( 'NONE',  ( 55.99999999999989342, 473.6663340069157471, -526.8058340126048051 ) ) ;
#2711 = CARTESIAN_POINT ( 'NONE',  ( 10.00000000000000000, 620.7506394335853201, -11.00000000000000000 ) ) ;
#2712 = CARTESIAN_POINT ( 'NONE',  ( 3.674999999999999822, 14.43750000000000000, 0.000000000000000000 ) ) ;
#2713 = CARTESIAN_POINT ( 'NONE',  ( 40.00000000000000000, 0.000000000000000000, -25.99999999999999645 ) ) ;
#2714 = CARTESIAN_POINT ( 'NONE',  ( 35.00000000000000711, 11.00000000000000000, -35.00000000000000711 ) ) ;
#2716 = ORIENTED_EDGE ( 'NONE', *, *, #5569, .T. ) ;
#2715 = ORIENTED_EDGE ( 'NONE', *, *, #4289, .T. ) ;
#2717 = CARTESIAN_POINT ( 'NONE',  ( 0.000000000000000000, 435.2933666400819561, -550.3792044179907634 ) ) ;
#2718 = CIRCLE ( 'NONE', #7956, 13.69540538389601991 ) ;
#2719 = CARTESIAN_POINT ( 'NONE',  ( 0.3822672831237738378, 286.0749473089381922, 37.32528944829249440 ) ) ;
#2720 = DIRECTION ( 'NONE',  ( 0.000000000000000000, 0.000000000000000000, 1.000000000000000000 ) ) ;
#2721 = CARTESIAN_POINT ( 'NONE',  ( 30.99999999999999645, 0.000000000000000000, 31.00000000000001066 ) ) ;
#2722 = VERTEX_POINT ( 'NONE', #10760 ) ;
#2723 = DIRECTION ( 'NONE',  ( -0.000000000000000000, -1.000000000000000000, -0.000000000000000000 ) ) ;
#2724 = AXIS2_PLACEMENT_3D ( 'NONE', #3453, #15118, #8606 ) ;
#2725 = CARTESIAN_POINT ( 'NONE',  ( -45.00000000000000000, 549.5810598491746077, -504.4200196135282113 ) ) ;
#2726 = EDGE_LOOP ( 'NONE', ( #9475, #6782, #9870, #8577 ) ) ;
#2727 = DIRECTION ( 'NONE',  ( -0.9998870921963913805, -0.01502673813723915709, 0.000000000000000000 ) ) ;
#2728 = EDGE_CURVE ( 'NONE', #12991, #7948, #2554, .T. ) ;
#2729 = CARTESIAN_POINT ( 'NONE',  ( 394.0000000000001137, 339.1725919290087745, -10.68226574335978718 ) ) ;
#2730 = VERTEX_POINT ( 'NONE', #14632 ) ;
#2731 = CARTESIAN_POINT ( 'NONE',  ( 2.799999999999999822, -13.30000000000000071, -1.628780242865979955E-15 ) ) ;
#2732 = CARTESIAN_POINT ( 'NONE',  ( 45.00000000000000000, 549.5810598491746077, -518.1154249974242703 ) ) ;
#2733 = ORIENTED_EDGE ( 'NONE', *, *, #4142, .T. ) ;
#2734 = EDGE_CURVE ( 'NONE', #12218, #9656, #8003, .T. ) ;
#2735 = FACE_OUTER_BOUND ( 'NONE', #13416, .T. ) ;
#2736 = MECHANICAL_DESIGN_GEOMETRIC_PRESENTATION_REPRESENTATION (  '', ( #2462 ), #7664 ) ;
#2737 = DIRECTION ( 'NONE',  ( 0.000000000000000000, 0.000000000000000000, -1.000000000000000000 ) ) ;
#2738 = AXIS2_PLACEMENT_3D ( 'NONE', #13478, #4293, #13566 ) ;
#2739 = DIRECTION ( 'NONE',  ( 1.000000000000000000, 0.000000000000000000, 0.000000000000000000 ) ) ;
#2740 = VERTEX_POINT ( 'NONE', #1662 ) ;
#2741 = PRODUCT_DEFINITION ( 'UNKNOWN', '', #14665, #9455 ) ;
#2742 = MANIFOLD_SOLID_BREP ( 'Cut-Extrude1', #9103 ) ;
#2743 = CARTESIAN_POINT ( 'NONE',  ( 0.000000000000000000, 66.00000000000000000, -5.741599279633704455E-16 ) ) ;
#2744 = UNCERTAINTY_MEASURE_WITH_UNIT (LENGTH_MEASURE( 1.000000000000000082E-05 ), #7740, 'distance_accuracy_value', 'NONE');
#2745 = LINE ( 'NONE', #2660, #8080 ) ;
#2746 = CARTESIAN_POINT ( 'NONE',  ( 31.99999999999998579, 10.00000000000000000, 22.99999999999999645 ) ) ;
#2747 = ORIENTED_EDGE ( 'NONE', *, *, #2763, .T. ) ;
#2748 = DIRECTION ( 'NONE',  ( 0.000000000000000000, 0.000000000000000000, -1.000000000000000000 ) ) ;
#2749 = DIRECTION ( 'NONE',  ( 0.000000000000000000, 0.000000000000000000, -1.000000000000000000 ) ) ;
#2750 = DIRECTION ( 'NONE',  ( 0.000000000000000000, 1.000000000000000000, 0.000000000000000000 ) ) ;
#2751 = EDGE_LOOP ( 'NONE', ( #10415, #9482 ) ) ;
#2752 = EDGE_CURVE ( 'NONE', #7889, #4822, #4072, .T. ) ;
#2753 = CIRCLE ( 'NONE', #14002, 13.69540538389601991 ) ;
#2754 = VECTOR ( 'NONE', #16109, 1000.000000000000000 ) ;
#2755 = ORIENTED_EDGE ( 'NONE', *, *, #2381, .F. ) ;
#2756 = ORIENTED_EDGE ( 'NONE', *, *, #7691, .F. ) ;
#2757 = DIRECTION ( 'NONE',  ( 0.000000000000000000, 0.000000000000000000, -1.000000000000000000 ) ) ;
#2758 = ORIENTED_EDGE ( 'NONE', *, *, #12966, .T. ) ;
#2759 = PRODUCT_CONTEXT ( 'NONE', #11158, 'mechanical' ) ;
#2760 = ORIENTED_EDGE ( 'NONE', *, *, #11941, .F. ) ;
#2761 = AXIS2_PLACEMENT_3D ( 'NONE', #1868, #12342, #15010 ) ;
#2762 = ORIENTED_EDGE ( 'NONE', *, *, #13411, .T. ) ;
#2763 = EDGE_CURVE ( 'NONE', #9809, #1865, #2289, .T. ) ;
#2764 = FACE_OUTER_BOUND ( 'NONE', #11390, .T. ) ;
#2765 = CARTESIAN_POINT ( 'NONE',  ( 40.00000000000003553, 3.000000000000000000, 26.00000000000000355 ) ) ;
#2766 = ORIENTED_EDGE ( 'NONE', *, *, #11170, .T. ) ;
#2767 = LINE ( 'NONE', #12906, #15992 ) ;
#2768 = EDGE_CURVE ( 'NONE', #1605, #7341, #9307, .T. ) ;
#2769 = FACE_OUTER_BOUND ( 'NONE', #1636, .T. ) ;
#2770 = ORIENTED_EDGE ( 'NONE', *, *, #12877, .T. ) ;
#2771 = ADVANCED_FACE ( 'NONE', ( #1495 ), #10075, .F. ) ;
#2772 = DIRECTION ( 'NONE',  ( 0.000000000000000000, -0.3420201433256626067, -0.9396926207859105373 ) ) ;
#2773 = ORIENTED_EDGE ( 'NONE', *, *, #1817, .T. ) ;
#2774 = DIRECTION ( 'NONE',  ( 1.000000000000000000, -0.000000000000000000, 0.000000000000000000 ) ) ;
#2775 = DIRECTION ( 'NONE',  ( -1.000000000000000000, 0.000000000000000000, -0.000000000000000000 ) ) ;
#2776 = ORIENTED_EDGE ( 'NONE', *, *, #11307, .F. ) ;
#2777 = FACE_OUTER_BOUND ( 'NONE', #15770, .T. ) ;
#2778 = ORIENTED_EDGE ( 'NONE', *, *, #15679, .T. ) ;
#2779 = DIRECTION ( 'NONE',  ( 0.000000000000000000, 0.000000000000000000, -1.000000000000000000 ) ) ;
#2780 = VECTOR ( 'NONE', #428, 1000.000000000000000 ) ;
#2781 = ORIENTED_EDGE ( 'NONE', *, *, #2898, .T. ) ;
#2782 = VERTEX_POINT ( 'NONE', #6018 ) ;
#2783 = PLANE ( 'NONE',  #4173 ) ;
#2784 = EDGE_CURVE ( 'NONE', #16870, #2164, #14917, .T. ) ;
#2785 = CARTESIAN_POINT ( 'NONE',  ( -55.99999999999989342, 523.2161522479893847, -590.5524132976893270 ) ) ;
#2786 = CARTESIAN_POINT ( 'NONE',  ( 394.0000000000001137, 339.4485271457185718, -110.7359021160857537 ) ) ;
#2787 = AXIS2_PLACEMENT_3D ( 'NONE', #15221, #960, #624 ) ;
#2788 = VERTEX_POINT ( 'NONE', #16594 ) ;
#2789 = PLANE ( 'NONE',  #4711 ) ;
#2790 = CARTESIAN_POINT ( 'NONE',  ( -31.00000000000002132, 10.00000000000000000, -31.00000000000000000 ) ) ;
#2791 = EDGE_CURVE ( 'NONE', #3811, #10491, #1908, .T. ) ;
#2792 = EDGE_CURVE ( 'NONE', #10404, #12229, #13855, .T. ) ;
#2793 = ADVANCED_FACE ( 'NONE', ( #4575 ), #9711, .F. ) ;
#2794 = CARTESIAN_POINT ( 'NONE',  ( 0.000000000000000000, 309.2289037985885898, -86.48019484660916589 ) ) ;
#2795 = ADVANCED_FACE ( 'NONE', ( #11351 ), #2081, .T. ) ;
#2796 = VECTOR ( 'NONE', #5655, 1000.000000000000000 ) ;
#2797 = VECTOR ( 'NONE', #6916, 1000.000000000000000 ) ;
#2798 = DIRECTION ( 'NONE',  ( -1.000000000000000000, 0.000000000000000000, 0.000000000000000000 ) ) ;
#2799 = DIRECTION ( 'NONE',  ( 1.000000000000000000, -0.000000000000000000, -0.000000000000000000 ) ) ;
#2800 = CYLINDRICAL_SURFACE ( 'NONE', #9442, 4.999999999999997335 ) ;
#2802 = ORIENTED_EDGE ( 'NONE', *, *, #5840, .T. ) ;
#2801 = ORIENTED_EDGE ( 'NONE', *, *, #7754, .T. ) ;
#2803 = AXIS2_PLACEMENT_3D ( 'NONE', #14261, #2484, #14515 ) ;
#2804 = CARTESIAN_POINT ( 'NONE',  ( 55.99999999999989342, 493.2350855268086320, -494.4847040861889127 ) ) ;
#2805 = CARTESIAN_POINT ( 'NONE',  ( 0.5437965083810563094, 286.1837381376100211, 37.26905881172037027 ) ) ;
#2806 = CIRCLE ( 'NONE', #9941, 3.300000000000000711 ) ;
#2807 = VECTOR ( 'NONE', #8114, 1000.000000000000000 ) ;
#2808 = CYLINDRICAL_SURFACE ( 'NONE', #1945, 4.999999999999997335 ) ;
#2809 = CARTESIAN_POINT ( 'NONE',  ( 414.6791312654406738, 352.3556387948262341, -6.736600000000000144 ) ) ;
#2810 = ORIENTED_EDGE ( 'NONE', *, *, #8213, .T. ) ;
#2811 = CARTESIAN_POINT ( 'NONE',  ( 36.99999999999999289, 10.00000000000000000, -22.99999999999999645 ) ) ;
#2812 = TOROIDAL_SURFACE ( 'NONE', #7188, 22.46376988133006236, 4.000164074322307250 ) ;
#2813 = DIRECTION ( 'NONE',  ( -1.000000000000000000, -0.000000000000000000, -0.000000000000000000 ) ) ;
#2814 = VERTEX_POINT ( 'NONE', #13942 ) ;
#2815 = DIRECTION ( 'NONE',  ( 0.000000000000000000, 1.000000000000000000, -1.224646799147353207E-16 ) ) ;
#2816 = EDGE_CURVE ( 'NONE', #4738, #8414, #7312, .T. ) ;
#2817 = DIRECTION ( 'NONE',  ( 0.000000000000000000, 0.000000000000000000, -1.000000000000000000 ) ) ;
#2818 = CARTESIAN_POINT ( 'NONE',  ( 7.000000000000000000, -17.52499999999999858, -2.146193515505736390E-15 ) ) ;
#2819 = VECTOR ( 'NONE', #3311, 1000.000000000000000 ) ;
#2820 = VECTOR ( 'NONE', #15102, 1000.000000000000000 ) ;
#2821 = SURFACE_STYLE_USAGE ( .BOTH. , #8227 ) ;
#2822 = CARTESIAN_POINT ( 'NONE',  ( 0.000000000000000000, -3.000000000000000000, 0.000000000000000000 ) ) ;
#2823 = ORIENTED_EDGE ( 'NONE', *, *, #16958, .T. ) ;
#2824 = CARTESIAN_POINT ( 'NONE',  ( 1.224646799147347044E-16, 38.00000000000000711, -0.9999999999999956701 ) ) ;
#2825 =( REPRESENTATION_RELATIONSHIP ('NONE','NONE', #9356, #11761 ) REPRESENTATION_RELATIONSHIP_WITH_TRANSFORMATION ( #12881 )SHAPE_REPRESENTATION_RELATIONSHIP( ) );
#2826 = AXIS2_PLACEMENT_3D ( 'NONE', #3209, #9480, #9651 ) ;
#2827 = LINE ( 'NONE', #3001, #9595 ) ;
#2828 = EDGE_CURVE ( 'NONE', #1155, #5033, #9150, .T. ) ;
#2829 = CARTESIAN_POINT ( 'NONE',  ( 54.99999999999999289, 645.2345343053611941, -411.3640676610526157 ) ) ;
#2830 = CIRCLE ( 'NONE', #5015, 14.27500000000000036 ) ;
#2831 = ORIENTED_EDGE ( 'NONE', *, *, #7355, .T. ) ;
#2832 = VECTOR ( 'NONE', #13543, 1000.000000000000000 ) ;
#2833 = AXIS2_PLACEMENT_3D ( 'NONE', #6884, #1757, #299 ) ;
#2834 = CARTESIAN_POINT ( 'NONE',  ( 31.00000000000000711, 0.000000000000000000, -30.99999999999999289 ) ) ;
#2835 = DIRECTION ( 'NONE',  ( 0.000000000000000000, 1.000000000000000000, 1.321694076934710402E-16 ) ) ;
#2836 = LINE ( 'NONE', #16148, #2076 ) ;
#2837 = EDGE_LOOP ( 'NONE', ( #10243, #3800, #13160, #15328 ) ) ;
#2838 = DIRECTION ( 'NONE',  ( -1.000000000000000000, -0.000000000000000000, -0.000000000000000000 ) ) ;
#2839 = CARTESIAN_POINT ( 'NONE',  ( -26.00000000000002132, 0.000000000000000000, -39.99999999999999289 ) ) ;
#2840 = CARTESIAN_POINT ( 'NONE',  ( 394.0000000000001137, 449.3157724647197142, 33.76061909850716347 ) ) ;
#2841 = ORIENTED_EDGE ( 'NONE', *, *, #700, .T. ) ;
#2842 = VECTOR ( 'NONE', #9030, 1000.000000000000000 ) ;
#2843 = DIRECTION ( 'NONE',  ( 0.000000000000000000, 0.000000000000000000, -1.000000000000000000 ) ) ;
#2844 = ORIENTED_EDGE ( 'NONE', *, *, #4440, .F. ) ;
#2845 = ORIENTED_EDGE ( 'NONE', *, *, #14744, .F. ) ;
#2846 = AXIS2_PLACEMENT_3D ( 'NONE', #8950, #14270, #2329 ) ;
#2847 = DIRECTION ( 'NONE',  ( -0.000000000000000000, -1.000000000000000000, -0.000000000000000000 ) ) ;
#2848 = TOROIDAL_SURFACE ( 'NONE', #12177, 4.695405383895982609, 9.000000000000000000 ) ;
#2849 = ORIENTED_EDGE ( 'NONE', *, *, #150, .T. ) ;
#2850 = AXIS2_PLACEMENT_3D ( 'NONE', #14194, #11695, #6434 ) ;
#2851 = ORIENTED_EDGE ( 'NONE', *, *, #13303, .F. ) ;
#2852 = VECTOR ( 'NONE', #4468, 1000.000000000000227 ) ;
#2853 = ORIENTED_EDGE ( 'NONE', *, *, #8241, .F. ) ;
#2854 = LINE ( 'NONE', #4065, #1416 ) ;
#2855 = DIRECTION ( 'NONE',  ( 0.7327934916262990317, 0.6804510993672779895, 0.000000000000000000 ) ) ;
#2856 = VECTOR ( 'NONE', #275, 1000.000000000000000 ) ;
#2857 = ORIENTED_EDGE ( 'NONE', *, *, #9913, .T. ) ;
#2858 = CARTESIAN_POINT ( 'NONE',  ( -40.00000000000000711, 0.000000000000000000, 26.00000000000000000 ) ) ;
#2859 = CARTESIAN_POINT ( 'NONE',  ( 3.500000000000000000, 0.000000000000000000, 0.000000000000000000 ) ) ;
#2860 = VERTEX_POINT ( 'NONE', #12561 ) ;
#2861 = VECTOR ( 'NONE', #2226, 1000.000000000000000 ) ;
#2862 = DIRECTION ( 'NONE',  ( -1.000000000000000000, -0.000000000000000000, -0.000000000000000000 ) ) ;
#2863 = ORIENTED_EDGE ( 'NONE', *, *, #870, .T. ) ;
#2864 = DIRECTION ( 'NONE',  ( 0.000000000000000000, 0.8660254037844424824, -0.4999999999999933387 ) ) ;
#2865 = DIRECTION ( 'NONE',  ( 0.000000000000000000, 0.000000000000000000, 1.000000000000000000 ) ) ;
#2866 = ORIENTED_EDGE ( 'NONE', *, *, #9612, .F. ) ;
#2867 = EDGE_CURVE ( 'NONE', #974, #15821, #723, .T. ) ;
#2868 = DIRECTION ( 'NONE',  ( 0.000000000000000000, 0.9848077530122061329, 0.1736481776669406840 ) ) ;
#2869 = VERTEX_POINT ( 'NONE', #3546 ) ;
#2870 = CYLINDRICAL_SURFACE ( 'NONE', #1531, 4.999999999999997335 ) ;
#2871 = TOROIDAL_SURFACE ( 'NONE', #16851, 4.695405383895982609, 9.000000000000000000 ) ;
#2872 = ORIENTED_EDGE ( 'NONE', *, *, #15269, .F. ) ;
#2873 = EDGE_CURVE ( 'NONE', #2243, #13962, #11187, .T. ) ;
#2874 = ORIENTED_EDGE ( 'NONE', *, *, #4948, .F. ) ;
#2875 = CARTESIAN_POINT ( 'NONE',  ( 6.649999999999999467, -18.17500000000000071, -2.225795557450314789E-15 ) ) ;
#2876 = AXIS2_PLACEMENT_3D ( 'NONE', #11153, #16467, #8495 ) ;
#2877 = CIRCLE ( 'NONE', #8087, 10.00000000000000178 ) ;
#2878 = LINE ( 'NONE', #8115, #1135 ) ;
#2879 = LINE ( 'NONE', #11898, #12990 ) ;
#2880 = ORIENTED_EDGE ( 'NONE', *, *, #13780, .T. ) ;
#2881 = LINE ( 'NONE', #16952, #9110 ) ;
#2882 = PLANE ( 'NONE',  #4211 ) ;
#2883 = CARTESIAN_POINT ( 'NONE',  ( 44.99999999999998579, 515.4878487013597805, -546.7230258972048205 ) ) ;
#2884 = LINE ( 'NONE', #1680, #3260 ) ;
#2885 = CARTESIAN_POINT ( 'NONE',  ( -19.00000000000001776, 8.000000000000000000, 40.00000000000000711 ) ) ;
#2886 = LINE ( 'NONE', #8031, #8579 ) ;
#2887 = EDGE_CURVE ( 'NONE', #1132, #3294, #7480, .T. ) ;
#2888 = CIRCLE ( 'NONE', #1245, 59.99999999999982947 ) ;
#2889 = FACE_OUTER_BOUND ( 'NONE', #11361, .T. ) ;
#2890 = DIRECTION ( 'NONE',  ( -1.000000000000000000, 0.000000000000000000, 0.000000000000000000 ) ) ;
#2892 = EDGE_LOOP ( 'NONE', ( #3299, #4726, #14440, #15560 ) ) ;
#2891 = VERTEX_POINT ( 'NONE', #16500 ) ;
#2893 = CARTESIAN_POINT ( 'NONE',  ( -23.00000000000002132, 0.000000000000000000, 31.00000000000003553 ) ) ;
#2894 = MANIFOLD_SOLID_BREP ( 'Cut-Extrude1', #8831 ) ;
#2895 = EDGE_CURVE ( 'NONE', #12820, #14413, #6670, .T. ) ;
#2896 = ADVANCED_FACE ( 'NONE', ( #12894 ), #16010, .T. ) ;
#2897 = ADVANCED_FACE ( 'NONE', ( #1298 ), #968, .T. ) ;
#2898 = EDGE_CURVE ( 'NONE', #4443, #7276, #7726, .T. ) ;
#2899 = CARTESIAN_POINT ( 'NONE',  ( 0.2077619023743854931, 289.4924457125955541, 37.56638074116236226 ) ) ;
#2900 = ADVANCED_FACE ( 'NONE', ( #1130 ), #9117, .T. ) ;
#2901 = LINE ( 'NONE', #12423, #9353 ) ;
#2902 = CARTESIAN_POINT ( 'NONE',  ( -45.00000000000000000, 559.9933750504617365, -560.4184312811007658 ) ) ;
#2903 = VECTOR ( 'NONE', #3461, 1000.000000000000000 ) ;
#2904 = ORIENTED_EDGE ( 'NONE', *, *, #6395, .F. ) ;
#2905 = AXIS2_PLACEMENT_3D ( 'NONE', #10829, #15880, #9363 ) ;
#2906 = CARTESIAN_POINT ( 'NONE',  ( 46.99999999999988631, 549.5810598491746077, -518.1154249974242703 ) ) ;
#2907 = DIRECTION ( 'NONE',  ( -1.071014023499572265E-32, 1.000000000000000000, -8.952264470854156086E-17 ) ) ;
#2908 = VERTEX_POINT ( 'NONE', #16917 ) ;
#2909 = CARTESIAN_POINT ( 'NONE',  ( -55.99999999999988631, 459.5014304922595443, -192.4166442068759579 ) ) ;
#2910 = DIRECTION ( 'NONE',  ( 0.000000000000000000, 0.000000000000000000, 1.000000000000000000 ) ) ;
#2911 = CARTESIAN_POINT ( 'NONE',  ( -36.00000000000000711, 10.00000000000000000, -22.00000000000000355 ) ) ;
#2912 = EDGE_LOOP ( 'NONE', ( #12136, #951, #15678, #3160, #9853, #725 ) ) ;
#2913 = CARTESIAN_POINT ( 'NONE',  ( 17.99999999999998579, 10.00000000000000000, -36.99999999999999289 ) ) ;
#2914 = CARTESIAN_POINT ( 'NONE',  ( 10.00000000000000000, 336.2713855965630501, -311.0652884549417081 ) ) ;
#2915 = CARTESIAN_POINT ( 'NONE',  ( 0.000000000000000000, 0.000000000000000000, 0.000000000000000000 ) ) ;
#2916 = VERTEX_POINT ( 'NONE', #14105 ) ;
#2917 = CARTESIAN_POINT ( 'NONE',  ( 10.00000000000000000, 226.8713558223388134, -346.2582248962859808 ) ) ;
#2918 = AXIS2_PLACEMENT_3D ( 'NONE', #5044, #3598, #15614 ) ;
#2919 = EDGE_CURVE ( 'NONE', #15508, #6970, #2241, .T. ) ;
#2920 = CARTESIAN_POINT ( 'NONE',  ( -26.00000000000001776, 0.000000000000000000, 31.00000000000003553 ) ) ;
#2921 = EDGE_CURVE ( 'NONE', #12389, #6110, #7468, .T. ) ;
#2922 = DIRECTION ( 'NONE',  ( 0.000000000000000000, 0.000000000000000000, -1.000000000000000000 ) ) ;
#2923 = ORIENTED_EDGE ( 'NONE', *, *, #1183, .T. ) ;
#2924 = DIRECTION ( 'NONE',  ( -1.000000000000000000, -0.000000000000000000, -0.000000000000000000 ) ) ;
#2925 = UNCERTAINTY_MEASURE_WITH_UNIT (LENGTH_MEASURE( 1.000000000000000082E-05 ), #7545, 'distance_accuracy_value', 'NONE');
#2926 = CYLINDRICAL_SURFACE ( 'NONE', #14680, 9.999999999999998224 ) ;
#2927 = VECTOR ( 'NONE', #14686, 1000.000000000000000 ) ;
#2928 = CARTESIAN_POINT ( 'NONE',  ( 1.347066989204613998E-15, 6.000000000000000000, 24.99999999999999645 ) ) ;
#2929 = EDGE_LOOP ( 'NONE', ( #6123, #1251, #3871, #3791 ) ) ;
#2930 = VECTOR ( 'NONE', #10851, 1000.000000000000000 ) ;
#2931 = CARTESIAN_POINT ( 'NONE',  ( 394.0000000000001137, 234.3157724647196289, -104.2090657433598011 ) ) ;
#2932 = PLANE ( 'NONE',  #15584 ) ;
#2933 = LINE ( 'NONE', #5488, #14159 ) ;
#2934 = EDGE_LOOP ( 'NONE', ( #8451, #11721, #14468, #7643 ) ) ;
#2935 = CARTESIAN_POINT ( 'NONE',  ( -33.99999999999997158, -20.00000000000000000, -22.99999999999999645 ) ) ;
#2936 = EDGE_LOOP ( 'NONE', ( #9491, #3975 ) ) ;
#2937 = APPLICATION_CONTEXT ( 'automotive_design' ) ;
#2938 = VERTEX_POINT ( 'NONE', #9034 ) ;
#2939 = LINE ( 'NONE', #9555, #3421 ) ;
#2940 = EDGE_LOOP ( 'NONE', ( #9216, #3098, #8494, #12237 ) ) ;
#2941 = SHAPE_DEFINITION_REPRESENTATION ( #5776, #9356 ) ;
#2942 = CIRCLE ( 'NONE', #3457, 9.000000000000007105 ) ;
#2943 = ORIENTED_EDGE ( 'NONE', *, *, #1261, .F. ) ;
#2944 = ORIENTED_EDGE ( 'NONE', *, *, #12222, .T. ) ;
#2945 = CARTESIAN_POINT ( 'NONE',  ( -36.00000000000000711, 6.000000000000000000, -22.00000000000000355 ) ) ;
#2946 = PLANE ( 'NONE',  #11635 ) ;
#2947 = ORIENTED_EDGE ( 'NONE', *, *, #16516, .F. ) ;
#2948 = FACE_OUTER_BOUND ( 'NONE', #4906, .T. ) ;
#2949 = DIRECTION ( 'NONE',  ( 0.000000000000000000, 0.000000000000000000, -1.000000000000000000 ) ) ;
#2950 = VERTEX_POINT ( 'NONE', #7558 ) ;
#2951 = VECTOR ( 'NONE', #5250, 1000.000000000000000 ) ;
#2952 = DIRECTION ( 'NONE',  ( 0.000000000000000000, 1.000000000000000000, 0.000000000000000000 ) ) ;
#2953 = ORIENTED_EDGE ( 'NONE', *, *, #13325, .T. ) ;
#2954 = LINE ( 'NONE', #11791, #2951 ) ;
#2955 = DIRECTION ( 'NONE',  ( -1.000000000000000000, 0.000000000000000000, 0.000000000000000000 ) ) ;
#2956 = VERTEX_POINT ( 'NONE', #15476 ) ;
#2957 = CARTESIAN_POINT ( 'NONE',  ( -46.99999999999988631, 523.2161522479893847, -590.5524132976893270 ) ) ;
#2958 = VERTEX_POINT ( 'NONE', #10403 ) ;
#2959 = DIRECTION ( 'NONE',  ( 0.3832643291392058282, 0.000000000000000000, 0.9236387031786154056 ) ) ;
#2960 = CARTESIAN_POINT ( 'NONE',  ( -40.00000000000000000, 68.00000000000000000, 26.00000000000000355 ) ) ;
#2961 = EDGE_LOOP ( 'NONE', ( #6567, #464, #297, #14177 ) ) ;
#2962 = ORIENTED_EDGE ( 'NONE', *, *, #13661, .T. ) ;
#2963 = DIRECTION ( 'NONE',  ( -0.000000000000000000, -1.000000000000000000, -0.000000000000000000 ) ) ;
#2964 = DIRECTION ( 'NONE',  ( 0.000000000000000000, 1.000000000000000000, 0.000000000000000000 ) ) ;
#2965 = FACE_OUTER_BOUND ( 'NONE', #3433, .T. ) ;
#2966 = EDGE_CURVE ( 'NONE', #7581, #4652, #4225, .T. ) ;
#2967 = LINE ( 'NONE', #4427, #2686 ) ;
#2968 = DIRECTION ( 'NONE',  ( -1.000000000000000000, 0.000000000000000000, 0.000000000000000000 ) ) ;
#2969 = CARTESIAN_POINT ( 'NONE',  ( 22.99999999999995737, 3.000000000000000000, -33.99999999999998579 ) ) ;
#2970 = DIRECTION ( 'NONE',  ( 1.000000000000000000, -0.000000000000000000, 0.000000000000000000 ) ) ;
#2971 = DIRECTION ( 'NONE',  ( 0.000000000000000000, 0.000000000000000000, 1.000000000000000000 ) ) ;
#2972 = CARTESIAN_POINT ( 'NONE',  ( 31.00000000000003908, 19.00000000000000000, -26.00000000000000355 ) ) ;
#2973 = EDGE_CURVE ( 'NONE', #1542, #13093, #5294, .T. ) ;
#2974 = DIRECTION ( 'NONE',  ( 1.000000000000000000, 0.000000000000000000, -0.000000000000000000 ) ) ;
#2975 = VECTOR ( 'NONE', #1773, 1000.000000000000227 ) ;
#2976 = FACE_OUTER_BOUND ( 'NONE', #9851, .T. ) ;
#2978 = ORIENTED_EDGE ( 'NONE', *, *, #15739, .T. ) ;
#2977 = VERTEX_POINT ( 'NONE', #14 ) ;
#2979 = DIRECTION ( 'NONE',  ( -1.000000000000000000, 0.000000000000000000, -0.000000000000000000 ) ) ;
#2980 = CARTESIAN_POINT ( 'NONE',  ( 0.5524412557578002314, 286.1517303826834109, 37.26585803622771209 ) ) ;
#2981 = CARTESIAN_POINT ( 'NONE',  ( 31.00000000000003553, 11.00000000000000000, 25.99999999999999645 ) ) ;
#2982 = CYLINDRICAL_SURFACE ( 'NONE', #12438, 15.25000000000000000 ) ;
#2983 = ORIENTED_EDGE ( 'NONE', *, *, #15479, .F. ) ;
#2984 = ADVANCED_FACE ( 'NONE', ( #11600 ), #5230, .F. ) ;
#2985 = AXIS2_PLACEMENT_3D ( 'NONE', #4628, #11083, #2057 ) ;
#2986 = EDGE_CURVE ( 'NONE', #5602, #1719, #7768, .T. ) ;
#2987 = DIRECTION ( 'NONE',  ( -0.000000000000000000, -1.000000000000000000, -0.000000000000000000 ) ) ;
#2988 = CARTESIAN_POINT ( 'NONE',  ( -55.99999999999989342, 549.5810598491749488, -570.6352214130889706 ) ) ;
#2989 = ORIENTED_EDGE ( 'NONE', *, *, #15059, .T. ) ;
#2990 = CARTESIAN_POINT ( 'NONE',  ( 394.0000000000001137, 449.3157724647197142, 33.76061909850716347 ) ) ;
#2991 = ADVANCED_FACE ( 'NONE', ( #6186 ), #11438, .T. ) ;
#2992 = LINE ( 'NONE', #4450, #1554 ) ;
#2993 = DIRECTION ( 'NONE',  ( -0.000000000000000000, -0.000000000000000000, 1.000000000000000000 ) ) ;
#2994 = ADVANCED_FACE ( 'NONE', ( #14356 ), #1219, .T. ) ;
#2995 = ADVANCED_FACE ( 'NONE', ( #10324 ), #15561, .F. ) ;
#2996 = DIRECTION ( 'NONE',  ( -1.000000000000000000, -0.000000000000000000, -0.000000000000000000 ) ) ;
#2997 = CARTESIAN_POINT ( 'NONE',  ( 29.68009836720079875, 352.3758082234937206, -17.00000000000000000 ) ) ;
#2998 = DIRECTION ( 'NONE',  ( -0.000000000000000000, 1.000000000000000000, -0.000000000000000000 ) ) ;
#2999 = ORIENTED_EDGE ( 'NONE', *, *, #6846, .T. ) ;
#3000 = DIRECTION ( 'NONE',  ( 1.000000000000000000, 0.000000000000000000, 0.000000000000000000 ) ) ;
#3001 = CARTESIAN_POINT ( 'NONE',  ( 22.99999999999995737, 0.000000000000000000, -33.99999999999998579 ) ) ;
#3002 = DIRECTION ( 'NONE',  ( 6.092845550116206908E-17, -0.09950371902098546772, 0.9950371902099904853 ) ) ;
#3003 = AXIS2_PLACEMENT_3D ( 'NONE', #517, #14778, #8233 ) ;
#3004 = VERTEX_POINT ( 'NONE', #6263 ) ;
#3005 = ADVANCED_FACE ( 'NONE', ( #16752 ), #4982, .T. ) ;
#3006 = MANIFOLD_SOLID_BREP ( 'Boss-Extrude4', #16496 ) ;
#3007 = FACE_OUTER_BOUND ( 'NONE', #16160, .T. ) ;
#3008 = CARTESIAN_POINT ( 'NONE',  ( -3.000000000000000000, -1.836909530733565148E-16, 12.50000000000000000 ) ) ;
#3009 = CARTESIAN_POINT ( 'NONE',  ( -31.00000000000006395, 8.000000000000000000, 20.99999999999998934 ) ) ;
#3010 = VERTEX_POINT ( 'NONE', #10920 ) ;
#3011 = CARTESIAN_POINT ( 'NONE',  ( 0.000000000000000000, 5.352861011586007481E-13, -75.00000000000599698 ) ) ;
#3012 = EDGE_CURVE ( 'NONE', #4223, #15448, #7982, .T. ) ;
#3013 = DIRECTION ( 'NONE',  ( -1.000000000000000000, -0.000000000000000000, -1.631319816340925608E-17 ) ) ;
#3014 = LINE ( 'NONE', #7036, #4300 ) ;
#3015 = VERTEX_POINT ( 'NONE', #12040 ) ;
#3016 = ADVANCED_BREP_SHAPE_REPRESENTATION ( '', ( #14078, #1488 ), #15488 ) ;
#3017 = EDGE_CURVE ( 'NONE', #14546, #3021, #13425, .T. ) ;
#3018 = EDGE_CURVE ( 'NONE', #9524, #15129, #16298, .T. ) ;
#3019 = EDGE_CURVE ( 'NONE', #10713, #6054, #2298, .T. ) ;
#3020 = ORIENTED_EDGE ( 'NONE', *, *, #11684, .T. ) ;
#3021 = VERTEX_POINT ( 'NONE', #4317 ) ;
#3022 = CIRCLE ( 'NONE', #15099, 4.695405383896011919 ) ;
#3023 = DIRECTION ( 'NONE',  ( -1.000000000000000000, -0.000000000000000000, 0.000000000000000000 ) ) ;
#3024 = ORIENTED_EDGE ( 'NONE', *, *, #7892, .T. ) ;
#3025 = PRODUCT_CONTEXT ( 'NONE', #3906, 'mechanical' ) ;
#3026 = AXIS2_PLACEMENT_3D ( 'NONE', #9017, #12873, #13998 ) ;
#3027 = PRODUCT_DEFINITION_SHAPE ( 'NONE', 'NONE',  #16969 ) ;
#3028 = EDGE_LOOP ( 'NONE', ( #11692, #5339, #443, #16483 ) ) ;
#3029 = VERTEX_POINT ( 'NONE', #13337 ) ;
#3030 = CARTESIAN_POINT ( 'NONE',  ( -31.00000000000005329, 0.000000000000000000, -26.00000000000000355 ) ) ;
#3031 = CARTESIAN_POINT ( 'NONE',  ( -55.99999999999989342, 549.5810598491749488, -575.3306267969850296 ) ) ;
#3032 = VECTOR ( 'NONE', #9204, 1000.000000000000000 ) ;
#3033 = ORIENTED_EDGE ( 'NONE', *, *, #6438, .F. ) ;
#3035 = DIRECTION ( 'NONE',  ( 0.000000000000000000, 0.000000000000000000, -1.000000000000000000 ) ) ;
#3034 = CONICAL_SURFACE ( 'NONE', #9057, 18.17500000000000071, 0.7483780475235185525 ) ;
#3036 = APPLICATION_CONTEXT ( 'automotive_design' ) ;
#3037 = CARTESIAN_POINT ( 'NONE',  ( 0.000000000000000000, 372.8685141053783241, -150.1198051533980049 ) ) ;
#3038 = ORIENTED_EDGE ( 'NONE', *, *, #12545, .F. ) ;
#3039 = EDGE_LOOP ( 'NONE', ( #2841, #1474, #10325, #16301 ) ) ;
#3040 = DIRECTION ( 'NONE',  ( -0.000000000000000000, -0.000000000000000000, 1.000000000000000000 ) ) ;
#3041 = DIRECTION ( 'NONE',  ( -1.000000000000000000, 0.000000000000000000, 0.000000000000000000 ) ) ;
#3042 = ORIENTED_EDGE ( 'NONE', *, *, #9516, .F. ) ;
#3043 = VERTEX_POINT ( 'NONE', #6785 ) ;
#3044 = CARTESIAN_POINT ( 'NONE',  ( 0.000000000000000000, 449.3157724647196005, -155.1251505852266632 ) ) ;
#3045 = VECTOR ( 'NONE', #14142, 1000.000000000000000 ) ;
#3046 = ORIENTED_EDGE ( 'NONE', *, *, #5385, .T. ) ;
#3047 = VERTEX_POINT ( 'NONE', #1472 ) ;
#3048 = DIRECTION ( 'NONE',  ( -0.000000000000000000, -1.000000000000000000, -0.000000000000000000 ) ) ;
#3049 = AXIS2_PLACEMENT_3D ( 'NONE', #4844, #16521, #7242 ) ;
#3050 = EDGE_CURVE ( 'NONE', #2162, #2891, #5314, .T. ) ;
#3051 = FACE_OUTER_BOUND ( 'NONE', #16554, .T. ) ;
#3052 = DIRECTION ( 'NONE',  ( -1.000000000000000000, -0.000000000000000000, 1.156482317317883755E-15 ) ) ;
#3053 = LINE ( 'NONE', #4592, #13117 ) ;
#3054 = CARTESIAN_POINT ( 'NONE',  ( 40.00000000000003553, 0.000000000000000000, 26.00000000000000355 ) ) ;
#3055 = CIRCLE ( 'NONE', #2498, 9.000000000000007105 ) ;
#3056 = ADVANCED_FACE ( 'NONE', ( #7899 ), #15813, .F. ) ;
#3057 = DIRECTION ( 'NONE',  ( 0.000000000000000000, 0.000000000000000000, 1.000000000000000000 ) ) ;
#3058 = DIRECTION ( 'NONE',  ( 0.000000000000000000, 0.000000000000000000, -1.000000000000000000 ) ) ;
#3059 = CARTESIAN_POINT ( 'NONE',  ( -55.99999999999989342, 523.2161522479888163, -498.1982331128240276 ) ) ;
#3060 = CARTESIAN_POINT ( 'NONE',  ( 20.99999999999996092, 3.000000000000000000, 35.00000000000000711 ) ) ;
#3061 = DIRECTION ( 'NONE',  ( -1.000000000000000000, -1.141265444721583757E-16, 0.000000000000000000 ) ) ;
#3062 = SURFACE_STYLE_FILL_AREA ( #14832 ) ;
#3064 = VERTEX_POINT ( 'NONE', #14792 ) ;
#3063 = ORIENTED_EDGE ( 'NONE', *, *, #11915, .F. ) ;
#3065 = CARTESIAN_POINT ( 'NONE',  ( 26.00000000000001066, 68.00000000000000000, -31.00000000000002487 ) ) ;
#3066 = PRODUCT_RELATED_PRODUCT_CATEGORY ( 'part', '', ( #12073 ) ) ;
#3067 = MANIFOLD_SOLID_BREP ( 'Cut-Extrude1', #3074 ) ;
#3068 = AXIS2_PLACEMENT_3D ( 'NONE', #11199, #12824, #14368 ) ;
#3069 = CARTESIAN_POINT ( 'NONE',  ( -1.745738565996369118, 288.6739674670197928, 37.61874632382036765 ) ) ;
#3070 = DIRECTION ( 'NONE',  ( 3.854941057726258312E-16, -0.000000000000000000, 1.000000000000000000 ) ) ;
#3071 = CARTESIAN_POINT ( 'NONE',  ( 31.00000000000006750, 19.00000000000000000, -21.00000000000000355 ) ) ;
#3072 = EDGE_CURVE ( 'NONE', #3004, #12389, #11908, .T. ) ;
#3073 = ORIENTED_EDGE ( 'NONE', *, *, #16355, .F. ) ;
#3074 = CLOSED_SHELL ( 'NONE', ( #9568, #11936, #15248, #10089, #12949, #388, #9047, #7148, #3517, #15438, #16140, #12624 ) ) ;
#3075 = DIRECTION ( 'NONE',  ( 0.000000000000000000, 0.000000000000000000, 1.000000000000000000 ) ) ;
#3076 = DIRECTION ( 'NONE',  ( 0.000000000000000000, 0.000000000000000000, 1.000000000000000000 ) ) ;
#3077 = ORIENTED_EDGE ( 'NONE', *, *, #5090, .F. ) ;
#3078 = DIRECTION ( 'NONE',  ( 0.000000000000000000, 0.3746065934159141242, -0.9271838545667866471 ) ) ;
#3079 = LINE ( 'NONE', #14847, #2927 ) ;
#3080 = CARTESIAN_POINT ( 'NONE',  ( 40.00000000000003553, 3.000000000000000000, -25.99999999999999645 ) ) ;
#3081 = CIRCLE ( 'NONE', #14048, 2.500000000000002220 ) ;
#3082 = CARTESIAN_POINT ( 'NONE',  ( -31.81980515339462912, 0.000000000000000000, -31.81980515339465043 ) ) ;
#3083 = FACE_BOUND ( 'NONE', #5692, .T. ) ;
#3084 = ORIENTED_EDGE ( 'NONE', *, *, #11492, .F. ) ;
#3085 = DIRECTION ( 'NONE',  ( -0.000000000000000000, -1.000000000000000000, 0.000000000000000000 ) ) ;
#3086 = EDGE_CURVE ( 'NONE', #11696, #452, #15034, .T. ) ;
#3087 = AXIS2_PLACEMENT_3D ( 'NONE', #8489, #12519, #11309 ) ;
#3088 = VECTOR ( 'NONE', #11986, 1000.000000000000000 ) ;
#3089 = CARTESIAN_POINT ( 'NONE',  ( 75.00000000000000000, 277.8092731128509740, -29.71049682360898103 ) ) ;
#3090 = CARTESIAN_POINT ( 'NONE',  ( -26.00000000000002132, 10.00000000000000000, -31.00000000000003553 ) ) ;
#3091 = AXIS2_PLACEMENT_3D ( 'NONE', #6239, #2386, #13989 ) ;
#3092 = EDGE_CURVE ( 'NONE', #15552, #9768, #530, .T. ) ;
#3093 = VERTEX_POINT ( 'NONE', #5755 ) ;
#3094 = MANIFOLD_SOLID_BREP ( 'Cut-Extrude1', #12930 ) ;
#3095 = DIRECTION ( 'NONE',  ( 1.000000000000000000, 0.000000000000000000, 0.000000000000000000 ) ) ;
#3096 = PRODUCT_DEFINITION_CONTEXT ( 'detailed design', #3586, 'design' ) ;
#3097 = DIRECTION ( 'NONE',  ( -1.000000000000000000, -0.000000000000000000, -0.000000000000000000 ) ) ;
#3098 = ORIENTED_EDGE ( 'NONE', *, *, #3197, .T. ) ;
#3099 = DIRECTION ( 'NONE',  ( 0.000000000000000000, 0.000000000000000000, -1.000000000000000000 ) ) ;
#3100 = CIRCLE ( 'NONE', #14894, 3.000000000000000000 ) ;
#3101 = DIRECTION ( 'NONE',  ( -0.000000000000000000, -1.000000000000000000, 0.000000000000000000 ) ) ;
#3102 = CARTESIAN_POINT ( 'NONE',  ( 394.0000000000001137, 339.1725919290084335, -110.6822657433597925 ) ) ;
#3103 = EDGE_LOOP ( 'NONE', ( #11244, #9389, #9401, #16411 ) ) ;
#3104 = CARTESIAN_POINT ( 'NONE',  ( -31.00000000000005684, 68.00000000000000000, 23.00000000000000355 ) ) ;
#3105 = ORIENTED_EDGE ( 'NONE', *, *, #4155, .F. ) ;
#3106 = ORIENTED_EDGE ( 'NONE', *, *, #587, .F. ) ;
#3107 = AXIS2_PLACEMENT_3D ( 'NONE', #421, #75, #9343 ) ;
#3108 = CARTESIAN_POINT ( 'NONE',  ( 5.950000000000000178, 0.000000000000000000, 0.000000000000000000 ) ) ;
#3109 = EDGE_CURVE ( 'NONE', #2235, #4506, #1975, .T. ) ;
#3110 = EDGE_LOOP ( 'NONE', ( #7861, #14209 ) ) ;
#3111 = DIRECTION ( 'NONE',  ( 0.000000000000000000, 1.000000000000000000, 0.000000000000000000 ) ) ;
#3112 = AXIS2_PLACEMENT_3D ( 'NONE', #6363, #11624, #7742 ) ;
#3113 = CIRCLE ( 'NONE', #7471, 4.695405383896011919 ) ;
#3114 = CIRCLE ( 'NONE', #5287, 12.65000000000000036 ) ;
#3115 = ORIENTED_EDGE ( 'NONE', *, *, #6555, .F. ) ;
#3116 = EDGE_CURVE ( 'NONE', #8783, #7005, #937, .T. ) ;
#3117 = DIRECTION ( 'NONE',  ( 1.000000000000000000, 0.000000000000000000, 0.000000000000000000 ) ) ;
#3118 = EDGE_CURVE ( 'NONE', #14799, #9375, #12733, .T. ) ;
#3119 = EDGE_CURVE ( 'NONE', #6145, #1948, #120, .T. ) ;
#3120 = ORIENTED_EDGE ( 'NONE', *, *, #13473, .F. ) ;
#3121 = EDGE_CURVE ( 'NONE', #4316, #4076, #12293, .T. ) ;
#3122 = FACE_BOUND ( 'NONE', #12220, .T. ) ;
#3123 = CARTESIAN_POINT ( 'NONE',  ( -150.0000000000000284, 620.7506394335853201, -11.00000000000000000 ) ) ;
#3124 = CIRCLE ( 'NONE', #919, 12.00000000000000178 ) ;
#3125 = ORIENTED_EDGE ( 'NONE', *, *, #9099, .T. ) ;
#3126 = CARTESIAN_POINT ( 'NONE',  ( -25.99999999999999645, 68.00000000000000000, 40.00000000000002132 ) ) ;
#3127 = DIRECTION ( 'NONE',  ( -0.000000000000000000, -0.000000000000000000, 1.000000000000000000 ) ) ;
#3128 = ORIENTED_EDGE ( 'NONE', *, *, #13080, .F. ) ;
#3129 = VECTOR ( 'NONE', #3626, 1000.000000000000000 ) ;
#3130 = AXIS2_PLACEMENT_3D ( 'NONE', #10417, #16932, #3891 ) ;
#3131 = DIRECTION ( 'NONE',  ( 0.000000000000000000, 0.000000000000000000, -1.000000000000000000 ) ) ;
#3132 = VECTOR ( 'NONE', #6636, 1000.000000000000000 ) ;
#3133 = ORIENTED_EDGE ( 'NONE', *, *, #12664, .T. ) ;
#3134 = LINE ( 'NONE', #16730, #4591 ) ;
#3135 = FACE_OUTER_BOUND ( 'NONE', #3568, .T. ) ;
#3136 = VERTEX_POINT ( 'NONE', #9969 ) ;
#3137 = VECTOR ( 'NONE', #10960, 1000.000000000000000 ) ;
#3138 = ORIENTED_EDGE ( 'NONE', *, *, #14332, .F. ) ;
#3139 = CARTESIAN_POINT ( 'NONE',  ( 23.66755185189983735, -100.1139154823664796, 76.44844828963165639 ) ) ;
#3140 = AXIS2_PLACEMENT_3D ( 'NONE', #6341, #11596, #5146 ) ;
#3141 = CARTESIAN_POINT ( 'NONE',  ( 17.00000000000000000, 355.3192028797624857, -44.71049682360899169 ) ) ;
#3142 = VERTEX_POINT ( 'NONE', #4713 ) ;
#3143 = PRESENTATION_LAYER_ASSIGNMENT (  '', '', ( #3955 ) ) ;
#3144 = ORIENTED_EDGE ( 'NONE', *, *, #9098, .T. ) ;
#3146 = CARTESIAN_POINT ( 'NONE',  ( 29.68009836720079875, 275.4439001176565398, -17.00000000000000355 ) ) ;
#3145 =( GEOMETRIC_REPRESENTATION_CONTEXT ( 3 ) GLOBAL_UNCERTAINTY_ASSIGNED_CONTEXT ( ( #8071 ) ) GLOBAL_UNIT_ASSIGNED_CONTEXT ( ( #8513, #7210, #11252 ) ) REPRESENTATION_CONTEXT ( 'NONE', 'WORKASPACE' ) );
#3147 = EDGE_CURVE ( 'NONE', #8007, #1605, #9727, .T. ) ;
#3148 = VECTOR ( 'NONE', #7996, 1000.000000000000000 ) ;
#3149 = DIRECTION ( 'NONE',  ( -1.000000000000000000, 0.000000000000000000, 0.000000000000000000 ) ) ;
#3150 = DIRECTION ( 'NONE',  ( 1.000000000000000000, 0.000000000000000000, 0.000000000000000000 ) ) ;
#3151 = CYLINDRICAL_SURFACE ( 'NONE', #11198, 2.999999999999999556 ) ;
#3152 = FACE_OUTER_BOUND ( 'NONE', #16754, .T. ) ;
#3153 = CARTESIAN_POINT ( 'NONE',  ( -2.220446049250313081E-13, 106.2500000000000142, 0.000000000000000000 ) ) ;
#3154 = DIRECTION ( 'NONE',  ( 1.000000000000000000, 0.000000000000000000, 0.000000000000000000 ) ) ;
#3155 = DIRECTION ( 'NONE',  ( -0.000000000000000000, 1.000000000000000000, -0.000000000000000000 ) ) ;
#3156 = DIRECTION ( 'NONE',  ( 0.000000000000000000, 0.000000000000000000, -1.000000000000000000 ) ) ;
#3157 = CARTESIAN_POINT ( 'NONE',  ( 46.99999999999988631, 473.6663340069158039, -561.9448123979092315 ) ) ;
#3158 = VECTOR ( 'NONE', #2835, 1000.000000000000000 ) ;
#3159 = CARTESIAN_POINT ( 'NONE',  ( 0.7365999999999783832, 260.4765148507123058, 287.1312267635910871 ) ) ;
#3161 = VERTEX_POINT ( 'NONE', #15209 ) ;
#3160 = ORIENTED_EDGE ( 'NONE', *, *, #3490, .T. ) ;
#3162 = CARTESIAN_POINT ( 'NONE',  ( 21.99999999999998224, 10.00000000000000000, -31.99999999999998579 ) ) ;
#3163 = CIRCLE ( 'NONE', #1224, 10.00000000000000178 ) ;
#3164 = MANIFOLD_SOLID_BREP ( 'Base-Flange1', #9370 ) ;
#3165 = DIRECTION ( 'NONE',  ( 0.000000000000000000, 0.000000000000000000, 1.000000000000000000 ) ) ;
#3166 = DIRECTION ( 'NONE',  ( 1.000000000000000000, 0.000000000000000000, 0.000000000000000000 ) ) ;
#3167 = DIRECTION ( 'NONE',  ( 1.000000000000000000, 0.000000000000000000, -0.000000000000000000 ) ) ;
#3168 = EDGE_LOOP ( 'NONE', ( #16077, #3905 ) ) ;
#3169 = DIRECTION ( 'NONE',  ( -0.000000000000000000, -1.000000000000000000, 0.000000000000000000 ) ) ;
#3170 = CARTESIAN_POINT ( 'NONE',  ( -55.99999999999989342, 493.2350855268092573, -571.5705369404290650 ) ) ;
#3171 = VERTEX_POINT ( 'NONE', #3779 ) ;
#3172 = CARTESIAN_POINT ( 'NONE',  ( 3.850000000000000089, 0.000000000000000000, -14.27500000000000036 ) ) ;
#3173 = CIRCLE ( 'NONE', #10838, 7.500000000000003553 ) ;
#3174 = CARTESIAN_POINT ( 'NONE',  ( 0.6401637624223318612, 192.7203252671974667, 37.23774918501624143 ) ) ;
#3175 = FACE_BOUND ( 'NONE', #5870, .T. ) ;
#3176 = PRODUCT_DEFINITION_SHAPE ( 'NONE', 'NONE',  #16972 ) ;
#3177 = LINE ( 'NONE', #4692, #14125 ) ;
#3178 = ORIENTED_EDGE ( 'NONE', *, *, #4661, .F. ) ;
#3179 = CYLINDRICAL_SURFACE ( 'NONE', #16047, 22.50000000000000000 ) ;
#3180 = CARTESIAN_POINT ( 'NONE',  ( 3.674999999999999822, -14.43750000000000000, -1.768083816268991068E-15 ) ) ;
#3181 = AXIS2_PLACEMENT_3D ( 'NONE', #14315, #6308, #10117 ) ;
#3182 = EDGE_LOOP ( 'NONE', ( #9359, #13565, #7138, #11443 ) ) ;
#3183 = MANIFOLD_SOLID_BREP ( 'Cut-Extrude1[2]', #5525 ) ;
#3184 = DIRECTION ( 'NONE',  ( 0.000000000000000000, 0.000000000000000000, 1.000000000000000000 ) ) ;
#3185 = EDGE_CURVE ( 'NONE', #10548, #12090, #3194, .T. ) ;
#3186 = CARTESIAN_POINT ( 'NONE',  ( -22.99999999999999645, 0.000000000000000000, 31.00000000000003908 ) ) ;
#3187 = ORIENTED_EDGE ( 'NONE', *, *, #11715, .F. ) ;
#3188 = LINE ( 'NONE', #13915, #16296 ) ;
#3189 = CARTESIAN_POINT ( 'NONE',  ( 25.99999999999998224, 10.00000000000000000, -32.99999999999999289 ) ) ;
#3190 = DIRECTION ( 'NONE',  ( -1.000000000000000000, -0.000000000000000000, -0.000000000000000000 ) ) ;
#3191 = VERTEX_POINT ( 'NONE', #11578 ) ;
#3192 = AXIS2_PLACEMENT_3D ( 'NONE', #11494, #1277, #16727 ) ;
#3193 = AXIS2_PLACEMENT_3D ( 'NONE', #10914, #14518, #1718 ) ;
#3194 = LINE ( 'NONE', #1110, #5763 ) ;
#3195 = ORIENTED_EDGE ( 'NONE', *, *, #7394, .F. ) ;
#3196 = ORIENTED_EDGE ( 'NONE', *, *, #2124, .T. ) ;
#3197 = EDGE_CURVE ( 'NONE', #14463, #3860, #14253, .T. ) ;
#3198 = CARTESIAN_POINT ( 'NONE',  ( -26.00000000000000000, 19.00000000000000000, -31.00000000000003908 ) ) ;
#3199 = APPLICATION_PROTOCOL_DEFINITION ( 'draft international standard', 'automotive_design', 1998, #2702 ) ;
#3200 = ORIENTED_EDGE ( 'NONE', *, *, #6686, .T. ) ;
#3201 = DIRECTION ( 'NONE',  ( -1.000000000000000000, -0.000000000000000000, -0.000000000000000000 ) ) ;
#3202 = VECTOR ( 'NONE', #10879, 1000.000000000000000 ) ;
#3203 = VERTEX_POINT ( 'NONE', #15368 ) ;
#3204 = AXIS2_PLACEMENT_3D ( 'NONE', #1028, #6240, #11489 ) ;
#3205 = DIRECTION ( 'NONE',  ( -0.000000000000000000, -1.000000000000000000, -0.000000000000000000 ) ) ;
#3206 = CARTESIAN_POINT ( 'NONE',  ( 30.99999999999999645, 68.00000000000000000, 31.00000000000001066 ) ) ;
#3207 = EDGE_CURVE ( 'NONE', #1561, #14012, #6168, .T. ) ;
#3208 = ORIENTED_EDGE ( 'NONE', *, *, #16835, .T. ) ;
#3209 = CARTESIAN_POINT ( 'NONE',  ( 0.000000000000000000, 16.00000000000000000, 0.000000000000000000 ) ) ;
#3210 = DIRECTION ( 'NONE',  ( 1.000000000000000000, 0.000000000000000000, 0.000000000000000000 ) ) ;
#3211 = ORIENTED_EDGE ( 'NONE', *, *, #10864, .F. ) ;
#3212 = CARTESIAN_POINT ( 'NONE',  ( 55.99999999999989342, 473.6663340069158039, -561.9448123979092315 ) ) ;
#3213 = EDGE_CURVE ( 'NONE', #3191, #6345, #832, .T. ) ;
#3214 = ORIENTED_EDGE ( 'NONE', *, *, #3516, .T. ) ;
#3215 = LINE ( 'NONE', #7541, #16275 ) ;
#3216 = EDGE_CURVE ( 'NONE', #10795, #5033, #13052, .T. ) ;
#3217 = ORIENTED_EDGE ( 'NONE', *, *, #13080, .T. ) ;
#3218 = CIRCLE ( 'NONE', #6214, 4.695405383896011919 ) ;
#3219 = ADVANCED_FACE ( 'NONE', ( #3857 ), #5052, .T. ) ;
#3220 = CIRCLE ( 'NONE', #7033, 13.69540538389601991 ) ;
#3221 = EDGE_CURVE ( 'NONE', #10479, #13963, #15544, .T. ) ;
#3222 = ORIENTED_EDGE ( 'NONE', *, *, #7306, .F. ) ;
#3223 = ORIENTED_EDGE ( 'NONE', *, *, #5649, .F. ) ;
#3224 = ORIENTED_EDGE ( 'NONE', *, *, #15611, .F. ) ;
#3225 = DIRECTION ( 'NONE',  ( 1.000000000000000000, 0.000000000000000000, 0.000000000000000000 ) ) ;
#3226 = CARTESIAN_POINT ( 'NONE',  ( -34.99999999999996447, 11.00000000000000000, -40.00000000000000711 ) ) ;
#3227 = PLANE ( 'NONE',  #14920 ) ;
#3228 = CARTESIAN_POINT ( 'NONE',  ( 0.000000000000000000, -3.000000000000000000, 0.000000000000000000 ) ) ;
#3229 = CYLINDRICAL_SURFACE ( 'NONE', #11074, 5.268482129199949959 ) ;
#3230 = DIRECTION ( 'NONE',  ( 1.000000000000000000, 0.000000000000000000, 0.000000000000000000 ) ) ;
#3231 = DIRECTION ( 'NONE',  ( 0.000000000000000000, 0.000000000000000000, -1.000000000000000000 ) ) ;
#3232 = EDGE_CURVE ( 'NONE', #16915, #11290, #3575, .T. ) ;
#3233 = ORIENTED_EDGE ( 'NONE', *, *, #13636, .F. ) ;
#3234 = DIRECTION ( 'NONE',  ( 1.000000000000000000, 0.000000000000000000, 0.000000000000000000 ) ) ;
#3235 = PLANE ( 'NONE',  #5003 ) ;
#3236 = EDGE_CURVE ( 'NONE', #221, #971, #7122, .T. ) ;
#3237 = EDGE_CURVE ( 'NONE', #856, #9116, #14082, .T. ) ;
#3238 = DIRECTION ( 'NONE',  ( 1.000000000000000000, 0.000000000000000000, 0.000000000000000000 ) ) ;
#3239 = DIRECTION ( 'NONE',  ( -1.000000000000000000, -0.000000000000000000, -0.000000000000000000 ) ) ;
#3241 = EDGE_LOOP ( 'NONE', ( #9996, #2414, #973, #8676 ) ) ;
#3240 = ORIENTED_EDGE ( 'NONE', *, *, #9098, .F. ) ;
#3242 = VECTOR ( 'NONE', #12690, 1000.000000000000000 ) ;
#3243 = CARTESIAN_POINT ( 'NONE',  ( 10.00000000000000000, 620.7506394335853201, 109.9999999999999858 ) ) ;
#3244 = MANIFOLD_SOLID_BREP ( 'Boss-Extrude3', #14305 ) ;
#3245 = FILL_AREA_STYLE_COLOUR ( '', #16239 ) ;
#3246 = CARTESIAN_POINT ( 'NONE',  ( -55.99999999999989342, 559.9933750504617365, -546.7230258972048205 ) ) ;
#3247 = FACE_BOUND ( 'NONE', #292, .T. ) ;
#3248 = ORIENTED_EDGE ( 'NONE', *, *, #10358, .F. ) ;
#3249 = LINE ( 'NONE', #5979, #2098 ) ;
#3250 = ORIENTED_EDGE ( 'NONE', *, *, #4969, .T. ) ;
#3251 = CARTESIAN_POINT ( 'NONE',  ( -2.601523022692215026, 61.50677485111217635, 9.137549538570182150 ) ) ;
#3252 = CIRCLE ( 'NONE', #7347, 7.500000000000000000 ) ;
#3253 = CARTESIAN_POINT ( 'NONE',  ( 6.299999999999999822, 0.000000000000000000, 0.000000000000000000 ) ) ;
#3254 = CARTESIAN_POINT ( 'NONE',  ( 0.000000000000000000, 0.000000000000000000, 0.000000000000000000 ) ) ;
#3255 = DIRECTION ( 'NONE',  ( 0.000000000000000000, 0.000000000000000000, 1.000000000000000000 ) ) ;
#3256 = LINE ( 'NONE', #1953, #8730 ) ;
#3257 = ORIENTED_EDGE ( 'NONE', *, *, #4665, .F. ) ;
#3258 = CARTESIAN_POINT ( 'NONE',  ( 54.99999999999999289, 172.2913238082672933, 146.1547335252150788 ) ) ;
#3259 = CARTESIAN_POINT ( 'NONE',  ( 22.99999999999999289, 0.000000000000000000, 37.00000000000002132 ) ) ;
#3260 = VECTOR ( 'NONE', #5538, 1000.000000000000000 ) ;
#3261 =( LENGTH_UNIT ( ) NAMED_UNIT ( * ) SI_UNIT ( .MILLI., .METRE. ) );
#3262 = EDGE_LOOP ( 'NONE', ( #907, #5182, #11693, #7882 ) ) ;
#3263 = LINE ( 'NONE', #11161, #3921 ) ;
#3264 = EDGE_CURVE ( 'NONE', #9092, #11763, #3610, .T. ) ;
#3265 = CARTESIAN_POINT ( 'NONE',  ( 35.99999999999999289, 6.000000000000000000, 17.99999999999998934 ) ) ;
#3266 = EDGE_LOOP ( 'NONE', ( #14732, #9213, #9311, #1895 ) ) ;
#3267 = CARTESIAN_POINT ( 'NONE',  ( -55.99999999999989342, 493.2350855268092573, -589.9613477082210693 ) ) ;
#3268 = CARTESIAN_POINT ( 'NONE',  ( 31.99999999999998579, 6.000000000000000000, 21.99999999999999645 ) ) ;
#3269 = DIRECTION ( 'NONE',  ( 1.000000000000000000, 0.000000000000000000, 0.000000000000000000 ) ) ;
#3270 = VERTEX_POINT ( 'NONE', #15954 ) ;
#3271 = EDGE_CURVE ( 'NONE', #8018, #7469, #8547, .T. ) ;
#3272 = VECTOR ( 'NONE', #3480, 1000.000000000000000 ) ;
#3273 = PRESENTATION_STYLE_ASSIGNMENT (( #12619 ) ) ;
#3274 = ORIENTED_EDGE ( 'NONE', *, *, #3092, .F. ) ;
#3275 = ORIENTED_EDGE ( 'NONE', *, *, #15059, .F. ) ;
#3276 = LINE ( 'NONE', #9974, #9185 ) ;
#3277 = PRODUCT_CONTEXT ( 'NONE', #6196, 'mechanical' ) ;
#3278 = AXIS2_PLACEMENT_3D ( 'NONE', #3394, #15150, #3057 ) ;
#3279 = PRODUCT_RELATED_PRODUCT_CATEGORY ( 'part', '', ( #8762 ) ) ;
#3280 = CARTESIAN_POINT ( 'NONE',  ( 0.000000000000000000, 0.000000000000000000, 0.000000000000000000 ) ) ;
#3281 = CYLINDRICAL_SURFACE ( 'NONE', #12882, 4.999999999999997335 ) ;
#3282 = VERTEX_POINT ( 'NONE', #4032 ) ;
#3283 = CYLINDRICAL_SURFACE ( 'NONE', #13766, 13.69540538389601991 ) ;
#3284 = DIRECTION ( 'NONE',  ( -0.000000000000000000, -1.000000000000000000, -0.000000000000000000 ) ) ;
#3285 = EDGE_CURVE ( 'NONE', #9217, #3723, #8226, .T. ) ;
#3286 = VERTEX_POINT ( 'NONE', #13134 ) ;
#3287 = CARTESIAN_POINT ( 'NONE',  ( 31.00000000000003553, 8.000000000000000000, 20.99999999999999289 ) ) ;
#3288 = DIRECTION ( 'NONE',  ( 0.000000000000000000, 0.09950371902100227373, 0.9950371902099888199 ) ) ;
#3289 = ORIENTED_EDGE ( 'NONE', *, *, #9055, .F. ) ;
#3290 = AXIS2_PLACEMENT_3D ( 'NONE', #3340, #8750, #13821 ) ;
#3291 = DIRECTION ( 'NONE',  ( 0.000000000000000000, -0.09950371902100807464, 0.9950371902099883759 ) ) ;
#3292 = VERTEX_POINT ( 'NONE', #14591 ) ;
#3293 = ORIENTED_EDGE ( 'NONE', *, *, #15495, .T. ) ;
#3294 = VERTEX_POINT ( 'NONE', #12099 ) ;
#3295 = EDGE_CURVE ( 'NONE', #16003, #14137, #5471, .T. ) ;
#3296 = VERTEX_POINT ( 'NONE', #15700 ) ;
#3297 = EDGE_CURVE ( 'NONE', #6332, #1567, #2517, .T. ) ;
#3298 = AXIS2_PLACEMENT_3D ( 'NONE', #6127, #574, #5800 ) ;
#3299 = ORIENTED_EDGE ( 'NONE', *, *, #1206, .F. ) ;
#3300 = CARTESIAN_POINT ( 'NONE',  ( -2.844582250340501162, 40.02709031926097083, 9.064464814046603536 ) ) ;
#3301 = AXIS2_PLACEMENT_3D ( 'NONE', #6405, #2642, #11665 ) ;
#3302 = LINE ( 'NONE', #16513, #8259 ) ;
#3303 = DIRECTION ( 'NONE',  ( -0.000000000000000000, -1.000000000000000000, -0.000000000000000000 ) ) ;
#3304 = EDGE_CURVE ( 'NONE', #15298, #6935, #4109, .T. ) ;
#3305 = DIRECTION ( 'NONE',  ( -0.000000000000000000, 1.000000000000000000, -0.000000000000000000 ) ) ;
#3306 = DIRECTION ( 'NONE',  ( 0.000000000000000000, -0.6930515690182840194, -0.7208880098054721852 ) ) ;
#3307 = CARTESIAN_POINT ( 'NONE',  ( -40.00000000000000711, 0.000000000000000000, -26.00000000000000000 ) ) ;
#3308 = DIRECTION ( 'NONE',  ( 0.000000000000000000, 0.000000000000000000, -1.000000000000000000 ) ) ;
#3309 = EDGE_LOOP ( 'NONE', ( #9892, #7063, #2673, #11481 ) ) ;
#3310 = LINE ( 'NONE', #8391, #8423 ) ;
#3311 = DIRECTION ( 'NONE',  ( 0.000000000000000000, 1.000000000000000000, 7.137148015447440312E-15 ) ) ;
#3312 = AXIS2_PLACEMENT_3D ( 'NONE', #2520, #1152, #2614 ) ;
#3313 = CARTESIAN_POINT ( 'NONE',  ( 0.000000000000000000, 381.0487089519832011, -80.00000000000332534 ) ) ;
#3314 = DIRECTION ( 'NONE',  ( -4.930380657631323236E-32, 0.09950371902099770793, -0.9950371902099891530 ) ) ;
#3316 = ORIENTED_EDGE ( 'NONE', *, *, #11176, .F. ) ;
#3315 = ORIENTED_EDGE ( 'NONE', *, *, #1128, .F. ) ;
#3317 = DIRECTION ( 'NONE',  ( -1.000000000000000000, -0.000000000000000000, -8.673617379884027583E-16 ) ) ;
#3318 = EDGE_CURVE ( 'NONE', #3004, #13474, #16507, .T. ) ;
#3319 = ORIENTED_EDGE ( 'NONE', *, *, #8992, .F. ) ;
#3320 = CARTESIAN_POINT ( 'NONE',  ( 55.99999999999989342, 523.2161522479893847, -604.2478186815853860 ) ) ;
#3321 = CARTESIAN_POINT ( 'NONE',  ( 37.18009836720080585, 275.4439001176564830, -75.00000000000000000 ) ) ;
#3322 = EDGE_CURVE ( 'NONE', #11217, #9633, #8008, .T. ) ;
#3323 = CARTESIAN_POINT ( 'NONE',  ( 5.950000000000000178, 0.000000000000000000, 0.000000000000000000 ) ) ;
#3324 = EDGE_CURVE ( 'NONE', #15724, #13772, #8059, .T. ) ;
#3325 = VECTOR ( 'NONE', #10889, 1000.000000000000000 ) ;
#3327 = ORIENTED_EDGE ( 'NONE', *, *, #5874, .F. ) ;
#3326 = EDGE_CURVE ( 'NONE', #1459, #3093, #5564, .T. ) ;
#3328 = EDGE_CURVE ( 'NONE', #2916, #10595, #16052, .T. ) ;
#3329 = DIRECTION ( 'NONE',  ( -0.000000000000000000, -0.000000000000000000, 1.000000000000000000 ) ) ;
#3330 = CARTESIAN_POINT ( 'NONE',  ( 5.425003271131650706, 12.64814671169700055, 0.000000000000000000 ) ) ;
#3331 = ORIENTED_EDGE ( 'NONE', *, *, #13751, .F. ) ;
#3332 = DIRECTION ( 'NONE',  ( 0.000000000000000000, 1.000000000000000000, 0.000000000000000000 ) ) ;
#3333 = DIRECTION ( 'NONE',  ( -1.000000000000000000, 0.000000000000000000, -0.000000000000000000 ) ) ;
#3334 = DIRECTION ( 'NONE',  ( -1.000000000000000000, 0.000000000000000000, 0.000000000000000000 ) ) ;
#3335 = DIRECTION ( 'NONE',  ( 0.000000000000000000, 0.000000000000000000, -1.000000000000000000 ) ) ;
#3336 = LINE ( 'NONE', #8746, #1591 ) ;
#3337 = ORIENTED_EDGE ( 'NONE', *, *, #5744, .F. ) ;
#3338 = AXIS2_PLACEMENT_3D ( 'NONE', #4261, #226, #1849 ) ;
#3339 = CARTESIAN_POINT ( 'NONE',  ( 10.00000000000000000, 309.2289037985890445, -143.5198051533984085 ) ) ;
#3340 = CARTESIAN_POINT ( 'NONE',  ( 1.399999999999999911, 0.000000000000000000, 0.000000000000000000 ) ) ;
#3341 = AXIS2_PLACEMENT_3D ( 'NONE', #10811, #1538, #6761 ) ;
#3342 = EDGE_LOOP ( 'NONE', ( #4361, #796, #9751, #15593, #13311, #7898 ) ) ;
#3343 = AXIS2_PLACEMENT_3D ( 'NONE', #12340, #7254, #10021 ) ;
#3344 = SURFACE_SIDE_STYLE ('',( #15023 ) ) ;
#3345 = VERTEX_POINT ( 'NONE', #9188 ) ;
#3346 = EDGE_CURVE ( 'NONE', #12951, #9574, #14421, .T. ) ;
#3347 = CARTESIAN_POINT ( 'NONE',  ( -22.99999999999999645, 68.00000000000000000, 31.00000000000003908 ) ) ;
#3348 = VECTOR ( 'NONE', #2154, 1000.000000000000000 ) ;
#3349 = CARTESIAN_POINT ( 'NONE',  ( 10.00000000000000000, 620.7506394335853201, -11.00000000000000000 ) ) ;
#3350 = ORIENTED_EDGE ( 'NONE', *, *, #2185, .F. ) ;
#3351 = DIRECTION ( 'NONE',  ( 1.000000000000000000, 0.000000000000000000, 0.000000000000000000 ) ) ;
#3352 = DIRECTION ( 'NONE',  ( 0.000000000000000000, -1.000000000000000000, -7.137148015447440312E-15 ) ) ;
#3353 = DIRECTION ( 'NONE',  ( -1.000000000000000000, -0.000000000000000000, -0.000000000000000000 ) ) ;
#3354 = ORIENTED_EDGE ( 'NONE', *, *, #16835, .F. ) ;
#3355 = VECTOR ( 'NONE', #5267, 1000.000000000000000 ) ;
#3356 = AXIS2_PLACEMENT_3D ( 'NONE', #15600, #11816, #7678 ) ;
#3357 = DIRECTION ( 'NONE',  ( 1.000000000000000000, -0.000000000000000000, -0.000000000000000000 ) ) ;
#3358 = AXIS2_PLACEMENT_3D ( 'NONE', #15923, #12243, #12570 ) ;
#3359 = ORIENTED_EDGE ( 'NONE', *, *, #7512, .F. ) ;
#3360 = EDGE_LOOP ( 'NONE', ( #12084, #15318, #11221, #10300 ) ) ;
#3361 = DIRECTION ( 'NONE',  ( -1.000000000000000000, 0.000000000000000000, -1.734723475976807094E-15 ) ) ;
#3362 = EDGE_CURVE ( 'NONE', #1542, #12590, #5304, .T. ) ;
#3363 = VECTOR ( 'NONE', #6508, 1000.000000000000000 ) ;
#3364 = LINE ( 'NONE', #7124, #10139 ) ;
#3365 = CIRCLE ( 'NONE', #5822, 187.4999999999998863 ) ;
#3366 = ORIENTED_EDGE ( 'NONE', *, *, #1993, .F. ) ;
#3367 = AXIS2_PLACEMENT_3D ( 'NONE', #10725, #437, #8420 ) ;
#3368 = CARTESIAN_POINT ( 'NONE',  ( 32.99999999999998579, 8.000000000000000000, 21.99999999999999645 ) ) ;
#3369 = CARTESIAN_POINT ( 'NONE',  ( 394.0000000000001137, 339.4485271457189128, -10.62862937063367852 ) ) ;
#3370 = ORIENTED_EDGE ( 'NONE', *, *, #15624, .T. ) ;
#3371 = PLANE ( 'NONE',  #7475 ) ;
#3372 = CARTESIAN_POINT ( 'NONE',  ( -20.99999999999999645, 19.00000000000000000, 31.00000000000003197 ) ) ;
#3373 = ORIENTED_EDGE ( 'NONE', *, *, #8528, .T. ) ;
#3374 = AXIS2_PLACEMENT_3D ( 'NONE', #4191, #6575, #9432 ) ;
#3375 = DIRECTION ( 'NONE',  ( 0.000000000000000000, 0.3420201433256757073, -0.9396926207859057634 ) ) ;
#3376 = VERTEX_POINT ( 'NONE', #9270 ) ;
#3377 = VERTEX_POINT ( 'NONE', #2731 ) ;
#3378 = AXIS2_PLACEMENT_3D ( 'NONE', #14509, #10467, #10559 ) ;
#3379 = AXIS2_PLACEMENT_3D ( 'NONE', #9779, #7257, #756 ) ;
#3380 = ORIENTED_EDGE ( 'NONE', *, *, #6661, .F. ) ;
#3381 =( LENGTH_UNIT ( ) NAMED_UNIT ( * ) SI_UNIT ( .MILLI., .METRE. ) );
#3382 = ORIENTED_EDGE ( 'NONE', *, *, #6132, .F. ) ;
#3383 = VECTOR ( 'NONE', #6198, 1000.000000000000000 ) ;
#3384 = ORIENTED_EDGE ( 'NONE', *, *, #1614, .F. ) ;
#3385 = CARTESIAN_POINT ( 'NONE',  ( -1.334572366541263433, 38.30595095619238322, 9.407584458684455697 ) ) ;
#3386 = DIRECTION ( 'NONE',  ( -0.000000000000000000, -1.000000000000000000, -0.000000000000000000 ) ) ;
#3387 = DIRECTION ( 'NONE',  ( 0.000000000000000000, 0.000000000000000000, -1.000000000000000000 ) ) ;
#3388 = CIRCLE ( 'NONE', #1161, 3.300000000000000711 ) ;
#3389 = CARTESIAN_POINT ( 'NONE',  ( -3.000000000000002220, 60.00000000000000711, 6.000000000000000000 ) ) ;
#3390 = DIRECTION ( 'NONE',  ( -0.000000000000000000, -1.000000000000000000, -0.000000000000000000 ) ) ;
#3391 = CIRCLE ( 'NONE', #6390, 15.14120580695350071 ) ;
#3392 = LINE ( 'NONE', #10006, #16804 ) ;
#3393 = EDGE_CURVE ( 'NONE', #10548, #777, #1450, .T. ) ;
#3394 = CARTESIAN_POINT ( 'NONE',  ( 0.000000000000000000, 240.0523724647196389, -104.2090657433598011 ) ) ;
#3395 = LINE ( 'NONE', #2099, #11587 ) ;
#3396 = ORIENTED_EDGE ( 'NONE', *, *, #280, .T. ) ;
#3397 = CARTESIAN_POINT ( 'NONE',  ( 0.000000000000000000, 104.2500000000000142, 3.000000000000000000 ) ) ;
#3398 = CARTESIAN_POINT ( 'NONE',  ( -18.00000000000001421, 6.000000000000000000, 40.00000000000000711 ) ) ;
#3399 = AXIS2_PLACEMENT_3D ( 'NONE', #8860, #1905, #14013 ) ;
#3400 = DIRECTION ( 'NONE',  ( -0.000000000000000000, -1.000000000000000000, -0.000000000000000000 ) ) ;
#3402 = ORIENTED_EDGE ( 'NONE', *, *, #4094, .F. ) ;
#3401 = ORIENTED_EDGE ( 'NONE', *, *, #13303, .T. ) ;
#3403 = AXIS2_PLACEMENT_3D ( 'NONE', #10236, #11858, #5677 ) ;
#3404 = EDGE_CURVE ( 'NONE', #6185, #1946, #14361, .T. ) ;
#3405 = DIRECTION ( 'NONE',  ( 1.000000000000000000, -0.000000000000000000, -0.000000000000000000 ) ) ;
#3406 = AXIS2_PLACEMENT_3D ( 'NONE', #563, #15145, #11275 ) ;
#3407 = ORIENTED_EDGE ( 'NONE', *, *, #11263, .T. ) ;
#3408 =( NAMED_UNIT ( * ) SI_UNIT ( $, .STERADIAN. ) SOLID_ANGLE_UNIT ( ) );
#3409 = CIRCLE ( 'NONE', #12725, 59.99999999999994316 ) ;
#3410 = CARTESIAN_POINT ( 'NONE',  ( -37.00000000000000000, 68.00000000000000000, 23.00000000000000355 ) ) ;
#3411 = CARTESIAN_POINT ( 'NONE',  ( -45.00000000000000000, 549.5810598491749488, -589.0260321808809749 ) ) ;
#3412 = VERTEX_POINT ( 'NONE', #4376 ) ;
#3413 = CARTESIAN_POINT ( 'NONE',  ( 39.99999999999999289, 8.000000000000000000, 26.00000000000000000 ) ) ;
#3414 = DIRECTION ( 'NONE',  ( 1.631319816340925608E-17, 0.000000000000000000, -1.000000000000000000 ) ) ;
#3416 = ORIENTED_EDGE ( 'NONE', *, *, #16440, .F. ) ;
#3415 = EDGE_CURVE ( 'NONE', #1870, #4809, #3388, .T. ) ;
#3417 = FACE_OUTER_BOUND ( 'NONE', #1749, .T. ) ;
#3418 = AXIS2_PLACEMENT_3D ( 'NONE', #795, #7049, #16339 ) ;
#3419 = CARTESIAN_POINT ( 'NONE',  ( -1.297668147409621886, 189.9512667226712779, 37.61531421653326390 ) ) ;
#3420 = CARTESIAN_POINT ( 'NONE',  ( 3.000000000000000000, 1.836909530733565148E-16, 22.00000000000000000 ) ) ;
#3421 = VECTOR ( 'NONE', #13340, 1000.000000000000114 ) ;
#3422 = DIRECTION ( 'NONE',  ( -0.000000000000000000, 0.000000000000000000, 1.000000000000000000 ) ) ;
#3423 = CARTESIAN_POINT ( 'NONE',  ( -46.99999999999988631, 493.2350855268086320, -503.4847040861888559 ) ) ;
#3424 = ORIENTED_EDGE ( 'NONE', *, *, #16120, .F. ) ;
#3425 = ADVANCED_FACE ( 'NONE', ( #13895 ), #13732, .T. ) ;
#3426 = EDGE_CURVE ( 'NONE', #14494, #13856, #429, .T. ) ;
#3427 = EDGE_CURVE ( 'NONE', #4760, #8117, #3365, .T. ) ;
#3428 = CARTESIAN_POINT ( 'NONE',  ( 55.99999999999989342, 549.5810598491746077, -518.1154249974242703 ) ) ;
#3429 = EDGE_CURVE ( 'NONE', #8130, #11672, #15421, .T. ) ;
#3430 = CARTESIAN_POINT ( 'NONE',  ( 10.00000000000000000, 306.0487089519837696, -155.0000000000038369 ) ) ;
#3431 = ORIENTED_EDGE ( 'NONE', *, *, #5653, .F. ) ;
#3432 = CARTESIAN_POINT ( 'NONE',  ( 32.99999999999998579, 8.000000000000000000, 25.99999999999999645 ) ) ;
#3433 = EDGE_LOOP ( 'NONE', ( #3223, #13105, #8245, #4845 ) ) ;
#3434 = AXIS2_PLACEMENT_3D ( 'NONE', #5823, #11232, #12605 ) ;
#3435 = DIRECTION ( 'NONE',  ( 1.000000000000000000, -0.000000000000000000, -0.000000000000000000 ) ) ;
#3436 = AXIS2_PLACEMENT_3D ( 'NONE', #12192, #4453, #15095 ) ;
#3437 = PLANE ( 'NONE',  #7024 ) ;
#3438 = ORIENTED_EDGE ( 'NONE', *, *, #2480, .F. ) ;
#3439 = FACE_OUTER_BOUND ( 'NONE', #15641, .T. ) ;
#3440 = CARTESIAN_POINT ( 'NONE',  ( -5.000000000000000000, 2.261139575227052682E-15, -18.46360580700775245 ) ) ;
#3441 = CYLINDRICAL_SURFACE ( 'NONE', #15530, 3.300000000000025135 ) ;
#3442 = VERTEX_POINT ( 'NONE', #1952 ) ;
#3443 = SURFACE_STYLE_FILL_AREA ( #9808 ) ;
#3444 = LINE ( 'NONE', #11422, #2671 ) ;
#3445 = ORIENTED_EDGE ( 'NONE', *, *, #11586, .T. ) ;
#3446 = EDGE_CURVE ( 'NONE', #7810, #9725, #2877, .T. ) ;
#3447 = VERTEX_POINT ( 'NONE', #7176 ) ;
#3448 = ADVANCED_FACE ( 'NONE', ( #12277 ), #2120, .T. ) ;
#3449 = CARTESIAN_POINT ( 'NONE',  ( -33.00000000000000000, 8.000000000000000000, -22.00000000000000355 ) ) ;
#3450 = CIRCLE ( 'NONE', #5636, 7.500000000000000000 ) ;
#3451 = EDGE_CURVE ( 'NONE', #4924, #7414, #11064, .T. ) ;
#3452 = APPLICATION_PROTOCOL_DEFINITION ( 'draft international standard', 'automotive_design', 1998, #13243 ) ;
#3453 = CARTESIAN_POINT ( 'NONE',  ( 0.000000000000000000, 226.8713558223388134, -346.2582248962859808 ) ) ;
#3454 = EDGE_LOOP ( 'NONE', ( #14871, #650, #16379, #3992, #1936 ) ) ;
#3455 = CARTESIAN_POINT ( 'NONE',  ( 55.99999999999989342, 493.2350855268092573, -571.5705369404290650 ) ) ;
#3456 = CARTESIAN_POINT ( 'NONE',  ( 0.000000000000000000, 339.1725919290087745, -9.945665743359786148 ) ) ;
#3457 = AXIS2_PLACEMENT_3D ( 'NONE', #546, #5858, #14885 ) ;
#3458 = ORIENTED_EDGE ( 'NONE', *, *, #225, .F. ) ;
#3459 = CIRCLE ( 'NONE', #12785, 7.500000000000007105 ) ;
#3460 = CARTESIAN_POINT ( 'NONE',  ( 56.72999999999999687, 289.4632308570087957, 37.52989836422092651 ) ) ;
#3461 = DIRECTION ( 'NONE',  ( -1.000000000000000000, -0.000000000000000000, -0.000000000000000000 ) ) ;
#3462 = VERTEX_POINT ( 'NONE', #8491 ) ;
#3463 = FILL_AREA_STYLE ('',( #15312 ) ) ;
#3464 = ORIENTED_EDGE ( 'NONE', *, *, #9846, .F. ) ;
#3465 = ORIENTED_EDGE ( 'NONE', *, *, #1703, .F. ) ;
#3466 = VERTEX_POINT ( 'NONE', #16387 ) ;
#3467 = CIRCLE ( 'NONE', #13067, 8.000000000000000000 ) ;
#3468 = CIRCLE ( 'NONE', #13346, 59.99999999999982947 ) ;
#3469 = ORIENTED_EDGE ( 'NONE', *, *, #2768, .F. ) ;
#3470 = ORIENTED_EDGE ( 'NONE', *, *, #8788, .F. ) ;
#3471 = LINE ( 'NONE', #14029, #71 ) ;
#3472 = DIRECTION ( 'NONE',  ( 0.000000000000000000, 0.000000000000000000, 1.000000000000000000 ) ) ;
#3473 = CARTESIAN_POINT ( 'NONE',  ( 35.99999999999999289, 6.000000000000000000, 17.99999999999998934 ) ) ;
#3474 = PLANE ( 'NONE',  #5149 ) ;
#3475 = FACE_OUTER_BOUND ( 'NONE', #12891, .T. ) ;
#3476 = LINE ( 'NONE', #11278, #13810 ) ;
#3477 = EDGE_CURVE ( 'NONE', #16779, #4249, #12354, .T. ) ;
#3478 = TOROIDAL_SURFACE ( 'NONE', #10330, 4.695405383895982609, 9.000000000000000000 ) ;
#3479 = CARTESIAN_POINT ( 'NONE',  ( -23.00000000000002132, 10.00000000000000000, 37.00000000000000711 ) ) ;
#3480 = DIRECTION ( 'NONE',  ( -0.000000000000000000, -0.000000000000000000, 1.000000000000000000 ) ) ;
#3481 = EDGE_LOOP ( 'NONE', ( #9399, #9345, #16241, #6259 ) ) ;
#3482 = CYLINDRICAL_SURFACE ( 'NONE', #11707, 25.25038683781155413 ) ;
#3483 = CARTESIAN_POINT ( 'NONE',  ( 10.00000000000000000, 309.2289037985885898, -86.48019484660916589 ) ) ;
#3484 = DIRECTION ( 'NONE',  ( -1.000000000000000000, -0.000000000000000000, -0.000000000000000000 ) ) ;
#3486 = EDGE_LOOP ( 'NONE', ( #16475, #8425 ) ) ;
#3485 = ORIENTED_EDGE ( 'NONE', *, *, #3264, .T. ) ;
#3487 = CARTESIAN_POINT ( 'NONE',  ( 46.99999999999988631, 493.2350855268086320, -508.1801094700848580 ) ) ;
#3488 = CIRCLE ( 'NONE', #6481, 4.999999999999997335 ) ;
#3489 = CARTESIAN_POINT ( 'NONE',  ( -46.99999999999988631, 549.5810598491749488, -575.3306267969850296 ) ) ;
#3490 = EDGE_CURVE ( 'NONE', #11680, #10468, #3177, .T. ) ;
#3491 = AXIS2_PLACEMENT_3D ( 'NONE', #16750, #9032, #6427 ) ;
#3492 = DIRECTION ( 'NONE',  ( -0.000000000000000000, -1.000000000000000000, -0.000000000000000000 ) ) ;
#3493 = LINE ( 'NONE', #12589, #16276 ) ;
#3494 = ORIENTED_EDGE ( 'NONE', *, *, #12637, .F. ) ;
#3495 = UNCERTAINTY_MEASURE_WITH_UNIT (LENGTH_MEASURE( 1.000000000000000082E-05 ), #7732, 'distance_accuracy_value', 'NONE');
#3496 = DIRECTION ( 'NONE',  ( -1.000000000000000000, 0.000000000000000000, 0.000000000000000000 ) ) ;
#3497 = ADVANCED_FACE ( 'NONE', ( #4616 ), #16307, .F. ) ;
#3498 = DIRECTION ( 'NONE',  ( -1.000000000000000000, -0.000000000000000000, -0.000000000000000000 ) ) ;
#3499 = ORIENTED_EDGE ( 'NONE', *, *, #16562, .F. ) ;
#3500 = CARTESIAN_POINT ( 'NONE',  ( -0.7808854937525574469, 62.90333651941379145, 9.469847369592788056 ) ) ;
#3501 = DIRECTION ( 'NONE',  ( 0.000000000000000000, 0.000000000000000000, -1.000000000000000000 ) ) ;
#3502 = CARTESIAN_POINT ( 'NONE',  ( -40.00000000000000711, 0.000000000000000000, 26.00000000000000000 ) ) ;
#3503 = AXIS2_PLACEMENT_3D ( 'NONE', #9970, #3606, #2222 ) ;
#3504 = PLANE ( 'NONE',  #10551 ) ;
#3505 = LINE ( 'NONE', #11312, #2399 ) ;
#3506 = ORIENTED_EDGE ( 'NONE', *, *, #1659, .T. ) ;
#3507 = DIRECTION ( 'NONE',  ( 0.000000000000000000, 0.000000000000000000, 1.000000000000000000 ) ) ;
#3508 = LINE ( 'NONE', #5826, #548 ) ;
#3509 = ADVANCED_FACE ( 'NONE', ( #1799 ), #9865, .F. ) ;
#3510 = EDGE_CURVE ( 'NONE', #2860, #13804, #13034, .T. ) ;
#3511 = DIRECTION ( 'NONE',  ( 0.000000000000000000, 0.000000000000000000, -1.000000000000000000 ) ) ;
#3512 = AXIS2_PLACEMENT_3D ( 'NONE', #8664, #2040, #13896 ) ;
#3513 = ORIENTED_EDGE ( 'NONE', *, *, #1039, .F. ) ;
#3514 = VECTOR ( 'NONE', #5227, 1000.000000000000000 ) ;
#3515 = CYLINDRICAL_SURFACE ( 'NONE', #1431, 9.999999999999994671 ) ;
#3516 = EDGE_CURVE ( 'NONE', #15290, #11828, #2039, .T. ) ;
#3517 = ADVANCED_FACE ( 'NONE', ( #11229 ), #16464, .F. ) ;
#3518 = CARTESIAN_POINT ( 'NONE',  ( 0.000000000000000000, 0.000000000000000000, 0.000000000000000000 ) ) ;
#3519 = EDGE_LOOP ( 'NONE', ( #3038, #9168, #3837, #14057 ) ) ;
#3520 = CARTESIAN_POINT ( 'NONE',  ( 34.99999999999997868, 0.000000000000000000, 40.00000000000000711 ) ) ;
#3521 = ADVANCED_FACE ( 'NONE', ( #8412 ), #13653, .T. ) ;
#3522 = DIRECTION ( 'NONE',  ( 0.000000000000000000, 0.000000000000000000, 1.000000000000000000 ) ) ;
#3523 = CARTESIAN_POINT ( 'NONE',  ( 21.00000000000000000, 19.00000000000000000, -35.00000000000000711 ) ) ;
#3524 = EDGE_LOOP ( 'NONE', ( #1937, #11015, #2187, #9553 ) ) ;
#3525 = FILL_AREA_STYLE ('',( #10054 ) ) ;
#3526 = LINE ( 'NONE', #8271, #10911 ) ;
#3527 = CARTESIAN_POINT ( 'NONE',  ( 394.0000000000001137, 240.0523724647196389, -104.2090657433598011 ) ) ;
#3528 = EDGE_LOOP ( 'NONE', ( #13846, #1579, #1612, #9578 ) ) ;
#3529 = ORIENTED_EDGE ( 'NONE', *, *, #13194, .F. ) ;
#3530 = LINE ( 'NONE', #4479, #16841 ) ;
#3531 = AXIS2_PLACEMENT_3D ( 'NONE', #11752, #10785, #9586 ) ;
#3532 = ITEM_DEFINED_TRANSFORMATION ( 'NONE', 'NONE', #2316,  #1488 ) ;
#3533 = ADVANCED_FACE ( 'NONE', ( #7522 ), #3504, .F. ) ;
#3534 = CYLINDRICAL_SURFACE ( 'NONE', #11002, 20.75209553982837463 ) ;
#3535 = ORIENTED_EDGE ( 'NONE', *, *, #16233, .F. ) ;
#3536 = DIRECTION ( 'NONE',  ( 0.000000000000000000, 0.000000000000000000, -1.000000000000000000 ) ) ;
#3537 = ADVANCED_FACE ( 'NONE', ( #12779 ), #15270, .T. ) ;
#3538 = CARTESIAN_POINT ( 'NONE',  ( 0.000000000000000000, 38.00000000000000711, -5.741599279633704455E-16 ) ) ;
#3539 = ADVANCED_FACE ( 'NONE', ( #13979 ), #15601, .F. ) ;
#3540 = EDGE_CURVE ( 'NONE', #9593, #14549, #3835, .T. ) ;
#3541 = ORIENTED_EDGE ( 'NONE', *, *, #1854, .T. ) ;
#3542 = CARTESIAN_POINT ( 'NONE',  ( -45.00000000000000000, 559.9933750504617365, -546.7230258972048205 ) ) ;
#3543 = EDGE_CURVE ( 'NONE', #199, #8018, #10196, .T. ) ;
#3544 = DIRECTION ( 'NONE',  ( -1.000000000000000000, -0.000000000000000000, 0.000000000000000000 ) ) ;
#3545 = VERTEX_POINT ( 'NONE', #1088 ) ;
#3546 = CARTESIAN_POINT ( 'NONE',  ( 3.850000000000000089, -14.27500000000000036, -1.768083816268991068E-15 ) ) ;
#3547 = ORIENTED_EDGE ( 'NONE', *, *, #10791, .F. ) ;
#3548 = ORIENTED_EDGE ( 'NONE', *, *, #10274, .F. ) ;
#3549 = VECTOR ( 'NONE', #10260, 1000.000000000000000 ) ;
#3550 = VERTEX_POINT ( 'NONE', #14310 ) ;
#3551 =( NAMED_UNIT ( * ) PLANE_ANGLE_UNIT ( ) SI_UNIT ( $, .RADIAN. ) );
#3552 = EDGE_LOOP ( 'NONE', ( #361, #12661, #2131, #12093 ) ) ;
#3553 = ORIENTED_EDGE ( 'NONE', *, *, #15795, .T. ) ;
#3554 = CARTESIAN_POINT ( 'NONE',  ( 56.72999999999999687, 264.4632308570091368, 287.5298983642207986 ) ) ;
#3555 = CARTESIAN_POINT ( 'NONE',  ( 10.00000000000000000, 226.8713558223388134, -358.7582248962859808 ) ) ;
#3556 = CARTESIAN_POINT ( 'NONE',  ( -31.00000000000003197, 0.000000000000000000, 26.00000000000000355 ) ) ;
#3557 = VECTOR ( 'NONE', #850, 1000.000000000000000 ) ;
#3558 = CARTESIAN_POINT ( 'NONE',  ( 0.000000000000000000, 65.20000000000000284, -5.741599279633704455E-16 ) ) ;
#3559 = DIRECTION ( 'NONE',  ( -0.000000000000000000, -1.000000000000000000, 0.000000000000000000 ) ) ;
#3560 = EDGE_CURVE ( 'NONE', #5152, #4052, #4785, .T. ) ;
#3561 = DIRECTION ( 'NONE',  ( 1.000000000000000000, 0.000000000000000000, -0.000000000000000000 ) ) ;
#3562 = CARTESIAN_POINT ( 'NONE',  ( 0.1969510947806087375, 63.00000000000001421, 9.500000000000003553 ) ) ;
#3563 = DIRECTION ( 'NONE',  ( 1.000000000000000000, 0.000000000000000000, -0.000000000000000000 ) ) ;
#3564 = ORIENTED_EDGE ( 'NONE', *, *, #9940, .T. ) ;
#3565 = CARTESIAN_POINT ( 'NONE',  ( -34.99999999999996447, 8.000000000000000000, -40.00000000000000711 ) ) ;
#3566 = LINE ( 'NONE', #2265, #14631 ) ;
#3567 = DIRECTION ( 'NONE',  ( 1.000000000000000000, 0.000000000000000000, 0.000000000000000000 ) ) ;
#3569 = VERTEX_POINT ( 'NONE', #11556 ) ;
#3568 = EDGE_LOOP ( 'NONE', ( #11467, #7560, #10308, #6605, #2305, #4000, #11131, #2331 ) ) ;
#3570 = CARTESIAN_POINT ( 'NONE',  ( -40.00000000000000711, 8.000000000000000000, -26.00000000000000000 ) ) ;
#3571 = AXIS2_PLACEMENT_3D ( 'NONE', #15346, #6224, #3759 ) ;
#3572 = EDGE_LOOP ( 'NONE', ( #7752, #5678 ) ) ;
#3573 = EDGE_CURVE ( 'NONE', #16578, #15837, #7685, .T. ) ;
#3574 = PRESENTATION_STYLE_ASSIGNMENT (( #4855 ) ) ;
#3575 = CIRCLE ( 'NONE', #4932, 14.59999999999999964 ) ;
#3576 = DIRECTION ( 'NONE',  ( 0.000000000000000000, -0.09950371902100807464, 0.9950371902099883759 ) ) ;
#3577 = LINE ( 'NONE', #14298, #1179 ) ;
#3578 = ORIENTED_EDGE ( 'NONE', *, *, #14271, .F. ) ;
#3579 = ADVANCED_FACE ( 'NONE', ( #7603 ), #10114, .F. ) ;
#3580 = CARTESIAN_POINT ( 'NONE',  ( -35.00000000000000000, 19.00000000000000000, 20.99999999999999289 ) ) ;
#3581 = AXIS2_PLACEMENT_3D ( 'NONE', #12811, #97, #15470 ) ;
#3582 = FACE_OUTER_BOUND ( 'NONE', #11884, .T. ) ;
#3583 = VERTEX_POINT ( 'NONE', #6062 ) ;
#3584 = DIRECTION ( 'NONE',  ( 0.000000000000000000, 0.000000000000000000, 1.000000000000000000 ) ) ;
#3585 = VECTOR ( 'NONE', #6738, 1000.000000000000000 ) ;
#3586 = APPLICATION_CONTEXT ( 'automotive_design' ) ;
#3587 = DIRECTION ( 'NONE',  ( 0.000000000000000000, 0.000000000000000000, -1.000000000000000000 ) ) ;
#3588 = DIRECTION ( 'NONE',  ( -0.000000000000000000, -0.000000000000000000, 1.000000000000000000 ) ) ;
#3589 = DIRECTION ( 'NONE',  ( 0.000000000000000000, -0.6930515690182841304, -0.7208880098054721852 ) ) ;
#3590 = DIRECTION ( 'NONE',  ( 0.000000000000000000, 0.000000000000000000, -1.000000000000000000 ) ) ;
#3591 = ORIENTED_EDGE ( 'NONE', *, *, #1549, .T. ) ;
#3592 = DIRECTION ( 'NONE',  ( -0.000000000000000000, -1.000000000000000000, -0.000000000000000000 ) ) ;
#3593 = AXIS2_PLACEMENT_3D ( 'NONE', #3410, #7506, #6051 ) ;
#3594 = CARTESIAN_POINT ( 'NONE',  ( 21.00000000000000000, 8.000000000000000000, -31.00000000000003908 ) ) ;
#3595 =( NAMED_UNIT ( * ) SI_UNIT ( $, .STERADIAN. ) SOLID_ANGLE_UNIT ( ) );
#3596 = EDGE_LOOP ( 'NONE', ( #10172, #14524, #11024, #8396 ) ) ;
#3597 = LINE ( 'NONE', #16803, #14887 ) ;
#3598 = DIRECTION ( 'NONE',  ( -1.000000000000000000, 0.000000000000000000, 0.000000000000000000 ) ) ;
#3599 = ORIENTED_EDGE ( 'NONE', *, *, #6284, .F. ) ;
#3600 = DIRECTION ( 'NONE',  ( -1.000000000000000000, -0.000000000000000000, 0.000000000000000000 ) ) ;
#3601 = LINE ( 'NONE', #4883, #6517 ) ;
#3602 = LINE ( 'NONE', #12539, #728 ) ;
#3603 = ORIENTED_EDGE ( 'NONE', *, *, #6875, .F. ) ;
#3604 = AXIS2_PLACEMENT_3D ( 'NONE', #8282, #5709, #16015 ) ;
#3605 = EDGE_CURVE ( 'NONE', #7059, #8520, #15741, .T. ) ;
#3606 = DIRECTION ( 'NONE',  ( -1.000000000000000000, 0.000000000000000000, 0.000000000000000000 ) ) ;
#3607 = FACE_OUTER_BOUND ( 'NONE', #13615, .T. ) ;
#3608 = ORIENTED_EDGE ( 'NONE', *, *, #15915, .T. ) ;
#3609 = DIRECTION ( 'NONE',  ( 0.000000000000000000, 0.000000000000000000, -1.000000000000000000 ) ) ;
#3610 = CIRCLE ( 'NONE', #7154, 8.000000000000000000 ) ;
#3611 = ADVANCED_FACE ( 'NONE', ( #15350 ), #16551, .T. ) ;
#3612 =( NAMED_UNIT ( * ) SI_UNIT ( $, .STERADIAN. ) SOLID_ANGLE_UNIT ( ) );
#3613 = DIRECTION ( 'NONE',  ( 0.000000000000000000, 0.000000000000000000, -1.000000000000000000 ) ) ;
#3614 = CIRCLE ( 'NONE', #8274, 10.00000000000000178 ) ;
#3615 = ORIENTED_EDGE ( 'NONE', *, *, #16868, .F. ) ;
#3616 = DIRECTION ( 'NONE',  ( 0.000000000000000000, 0.000000000000000000, 1.000000000000000000 ) ) ;
#3617 = LINE ( 'NONE', #2232, #7234 ) ;
#3618 = AXIS2_PLACEMENT_3D ( 'NONE', #4378, #4298, #14689 ) ;
#3619 = ORIENTED_EDGE ( 'NONE', *, *, #5470, .F. ) ;
#3620 = CARTESIAN_POINT ( 'NONE',  ( 22.99999999999998224, 10.00000000000000000, 37.00000000000000711 ) ) ;
#3621 = CLOSED_SHELL ( 'NONE', ( #15705, #13817, #1802, #5818, #7108, #2056, #4178, #14957, #10768, #11194, #12314, #10129, #15892, #8156, #6930, #1737, #2991, #171, #8174, #12550 ) ) ;
#3622 = AXIS2_PLACEMENT_3D ( 'NONE', #5036, #5124, #7867 ) ;
#3623 = CARTESIAN_POINT ( 'NONE',  ( 37.00000000000000000, 68.00000000000000000, -23.00000000000000000 ) ) ;
#3624 = EDGE_LOOP ( 'NONE', ( #9559, #5456, #7790, #15729 ) ) ;
#3625 = EDGE_CURVE ( 'NONE', #1459, #6709, #14062, .T. ) ;
#3626 = DIRECTION ( 'NONE',  ( 1.000000000000000000, -0.000000000000000000, -0.000000000000000000 ) ) ;
#3627 = VERTEX_POINT ( 'NONE', #2292 ) ;
#3628 = ORIENTED_EDGE ( 'NONE', *, *, #14796, .F. ) ;
#3629 = AXIS2_PLACEMENT_3D ( 'NONE', #13827, #4798, #9960 ) ;
#3630 = DIRECTION ( 'NONE',  ( -0.000000000000000000, 1.000000000000000000, -0.000000000000000000 ) ) ;
#3631 = EDGE_LOOP ( 'NONE', ( #8153, #14947 ) ) ;
#3632 = ADVANCED_FACE ( 'NONE', ( #14232 ), #1013, .F. ) ;
#3633 = DIRECTION ( 'NONE',  ( 0.000000000000000000, 0.000000000000000000, 1.000000000000000000 ) ) ;
#3634 = EDGE_CURVE ( 'NONE', #10263, #1429, #15432, .T. ) ;
#3635 = ADVANCED_FACE ( 'NONE', ( #6389 ), #3763, .T. ) ;
#3636 = ADVANCED_FACE ( 'NONE', ( #5117 ), #3923, .T. ) ;
#3637 = AXIS2_PLACEMENT_3D ( 'NONE', #999, #6291, #6215 ) ;
#3638 = ORIENTED_EDGE ( 'NONE', *, *, #485, .F. ) ;
#3639 = EDGE_LOOP ( 'NONE', ( #15500, #15284, #10446, #9907 ) ) ;
#3640 = FACE_OUTER_BOUND ( 'NONE', #7372, .T. ) ;
#3641 = CARTESIAN_POINT ( 'NONE',  ( -31.00000000000002842, 3.000000000000000000, 31.00000000000000000 ) ) ;
#3642 = CIRCLE ( 'NONE', #13245, 8.000000000000000000 ) ;
#3643 = DIRECTION ( 'NONE',  ( 0.000000000000000000, 0.000000000000000000, 1.000000000000000000 ) ) ;
#3644 = CARTESIAN_POINT ( 'NONE',  ( 0.000000000000000000, -3.000000000000000000, 35.00000000000000711 ) ) ;
#3645 = CARTESIAN_POINT ( 'NONE',  ( 25.99999999999999645, 68.00000000000000000, -39.99999999999999289 ) ) ;
#3646 = DIRECTION ( 'NONE',  ( -0.000000000000000000, -1.000000000000000000, 0.000000000000000000 ) ) ;
#3647 = DIRECTION ( 'NONE',  ( -1.000000000000000000, 0.000000000000000000, -0.000000000000000000 ) ) ;
#3648 = VECTOR ( 'NONE', #3511, 1000.000000000000000 ) ;
#3649 = EDGE_LOOP ( 'NONE', ( #333, #8327, #4035, #5418 ) ) ;
#3650 = CARTESIAN_POINT ( 'NONE',  ( 46.99999999999988631, 473.6663340069158039, -561.9448123979092315 ) ) ;
#3651 = DIRECTION ( 'NONE',  ( -1.000000000000000000, -0.000000000000000000, -0.000000000000000000 ) ) ;
#3652 = ORIENTED_EDGE ( 'NONE', *, *, #8341, .T. ) ;
#3653 = DIRECTION ( 'NONE',  ( -1.000000000000000000, -0.000000000000000000, -0.000000000000000000 ) ) ;
#3655 = EDGE_LOOP ( 'NONE', ( #3384, #15512, #6964, #8620 ) ) ;
#3654 = EDGE_LOOP ( 'NONE', ( #12440, #5094, #1321, #1730 ) ) ;
#3656 = AXIS2_PLACEMENT_3D ( 'NONE', #7999, #11619, #15737 ) ;
#3657 = CARTESIAN_POINT ( 'NONE',  ( 23.00000000000000711, 0.000000000000000000, -36.99999999999999289 ) ) ;
#3658 = ADVANCED_FACE ( 'NONE', ( #1259, #9165, #2889 ), #5454, .F. ) ;
#3659 = ORIENTED_EDGE ( 'NONE', *, *, #2060, .T. ) ;
#3660 = CIRCLE ( 'NONE', #14903, 3.000000000000000000 ) ;
#3662 = FILL_AREA_STYLE ('',( #15587 ) ) ;
#3661 = AXIS2_PLACEMENT_3D ( 'NONE', #6335, #10315, #15555 ) ;
#3663 = AXIS2_PLACEMENT_3D ( 'NONE', #254, #14688, #8317 ) ;
#3664 = CARTESIAN_POINT ( 'NONE',  ( 0.000000000000000000, 240.0523724647196389, -17.15546574335979813 ) ) ;
#3665 = FACE_OUTER_BOUND ( 'NONE', #1407, .T. ) ;
#3666 = ORIENTED_EDGE ( 'NONE', *, *, #13074, .T. ) ;
#3667 = UNCERTAINTY_MEASURE_WITH_UNIT (LENGTH_MEASURE( 1.000000000000000082E-05 ), #15870, 'distance_accuracy_value', 'NONE');
#3668 = DIRECTION ( 'NONE',  ( 1.000000000000000000, -0.000000000000000000, -0.000000000000000000 ) ) ;
#3669 = VECTOR ( 'NONE', #14100, 1000.000000000000000 ) ;
#3670 = EDGE_LOOP ( 'NONE', ( #1807, #12757, #2186, #8949 ) ) ;
#3671 = DIRECTION ( 'NONE',  ( 0.000000000000000000, 0.000000000000000000, 1.000000000000000000 ) ) ;
#3672 = FACE_BOUND ( 'NONE', #15014, .T. ) ;
#3673 = DIRECTION ( 'NONE',  ( 0.9998870921963913805, 0.01502673813723916403, 0.000000000000000000 ) ) ;
#3674 = COLOUR_RGB ( '', 0.66274510, 0.83137255, 0.94901961) ;
#3675 = AXIS2_PLACEMENT_3D ( 'NONE', #16437, #7147, #896 ) ;
#3676 = DIRECTION ( 'NONE',  ( 0.000000000000000000, 0.000000000000000000, -1.000000000000000000 ) ) ;
#3677 = VECTOR ( 'NONE', #10870, 1000.000000000000000 ) ;
#3678 = CARTESIAN_POINT ( 'NONE',  ( -36.00000000000000711, 8.000000000000000000, -22.00000000000000355 ) ) ;
#3679 = EDGE_LOOP ( 'NONE', ( #878, #8437, #3274, #10127, #7064, #7738 ) ) ;
#3680 = CARTESIAN_POINT ( 'NONE',  ( 31.00000000000003553, 0.000000000000000000, -23.00000000000000000 ) ) ;
#3681 = AXIS2_PLACEMENT_3D ( 'NONE', #5046, #10461, #3775 ) ;
#3682 = DIRECTION ( 'NONE',  ( -1.000000000000000000, -0.000000000000000000, -0.000000000000000000 ) ) ;
#3683 = CARTESIAN_POINT ( 'NONE',  ( -36.00000000000000711, 10.00000000000000000, -19.00000000000000000 ) ) ;
#3684 = ORIENTED_EDGE ( 'NONE', *, *, #59, .F. ) ;
#3685 = CIRCLE ( 'NONE', #13844, 10.00000000000000178 ) ;
#3686 = CARTESIAN_POINT ( 'NONE',  ( -31.00000000000002132, 0.000000000000000000, -31.00000000000000000 ) ) ;
#3687 = CARTESIAN_POINT ( 'NONE',  ( 4.469960816887838430E-15, 50.00000000000000000, 36.50000000000000000 ) ) ;
#3688 = ORIENTED_EDGE ( 'NONE', *, *, #6555, .T. ) ;
#3689 = CARTESIAN_POINT ( 'NONE',  ( 55.99999999999989342, 473.6663340069158039, -548.2494070140132862 ) ) ;
#3690 = VECTOR ( 'NONE', #707, 1000.000000000000000 ) ;
#3691 = DIRECTION ( 'NONE',  ( 1.000000000000000000, 0.000000000000000000, 0.000000000000000000 ) ) ;
#3692 = CARTESIAN_POINT ( 'NONE',  ( 0.000000000000000000, 309.2289037985885898, -83.18019484660915452 ) ) ;
#3693 = ORIENTED_EDGE ( 'NONE', *, *, #12414, .F. ) ;
#3694 = PRODUCT ( 'Part9^Assem2', 'Part9^Assem2', '', ( #10840 ) ) ;
#3695 = DIRECTION ( 'NONE',  ( 0.000000000000000000, 0.6427876096865299260, 0.7660444431189857850 ) ) ;
#3696 = LINE ( 'NONE', #8934, #11449 ) ;
#3697 = CARTESIAN_POINT ( 'NONE',  ( -2.764312543581500581, 287.4577225941200140, 37.59778641568931334 ) ) ;
#3698 = ORIENTED_EDGE ( 'NONE', *, *, #15679, .F. ) ;
#3699 = CARTESIAN_POINT ( 'NONE',  ( 17.00000000000000711, 277.8092731128509740, -37.21049682360897748 ) ) ;
#3700 = AXIS2_PLACEMENT_3D ( 'NONE', #3881, #5078, #11523 ) ;
#3701 = AXIS2_PLACEMENT_3D ( 'NONE', #10228, #15467, #3708 ) ;
#3702 = CONTEXT_DEPENDENT_SHAPE_REPRESENTATION ( #8096, #4268 ) ;
#3703 =( NAMED_UNIT ( * ) PLANE_ANGLE_UNIT ( ) SI_UNIT ( $, .RADIAN. ) );
#3704 = VECTOR ( 'NONE', #1625, 1000.000000000000000 ) ;
#3705 = VERTEX_POINT ( 'NONE', #10792 ) ;
#3706 = EDGE_CURVE ( 'NONE', #11572, #11419, #9252, .T. ) ;
#3707 = CARTESIAN_POINT ( 'NONE',  ( 30.99999999999999645, 0.000000000000000000, 26.00000000000000355 ) ) ;
#3708 = DIRECTION ( 'NONE',  ( 0.000000000000000000, 0.000000000000000000, -1.000000000000000000 ) ) ;
#3709 = FACE_OUTER_BOUND ( 'NONE', #11271, .T. ) ;
#3710 = ORIENTED_EDGE ( 'NONE', *, *, #14233, .F. ) ;
#3711 = CARTESIAN_POINT ( 'NONE',  ( -3.269999999998768114, 193.4898140233619017, 37.52989836422146652 ) ) ;
#3712 = ADVANCED_FACE ( 'NONE', ( #12081 ), #1602, .T. ) ;
#3713 = FACE_OUTER_BOUND ( 'NONE', #4136, .T. ) ;
#3714 = EDGE_LOOP ( 'NONE', ( #282, #10853 ) ) ;
#3715 = ADVANCED_FACE ( 'NONE', ( #319 ), #4093, .F. ) ;
#3716 = VECTOR ( 'NONE', #15006, 1000.000000000000000 ) ;
#3717 = VERTEX_POINT ( 'NONE', #10700 ) ;
#3718 = ORIENTED_EDGE ( 'NONE', *, *, #2144, .T. ) ;
#3719 = LINE ( 'NONE', #7561, #6678 ) ;
#3720 = ORIENTED_EDGE ( 'NONE', *, *, #1102, .F. ) ;
#3721 = DIRECTION ( 'NONE',  ( -3.491481338843182265E-15, -1.000000000000000000, -6.982962677686243045E-15 ) ) ;
#3722 = VERTEX_POINT ( 'NONE', #2539 ) ;
#3723 = VERTEX_POINT ( 'NONE', #16962 ) ;
#3724 = ADVANCED_FACE ( 'NONE', ( #1428 ), #60, .F. ) ;
#3725 = AXIS2_PLACEMENT_3D ( 'NONE', #14139, #12841, #11542 ) ;
#3726 = EDGE_CURVE ( 'NONE', #15077, #15661, #15768, .T. ) ;
#3727 = CARTESIAN_POINT ( 'NONE',  ( 4.025000000000000355, 17.52499999999999858, 0.000000000000000000 ) ) ;
#3728 = LINE ( 'NONE', #6272, #5030 ) ;
#3729 = ORIENTED_EDGE ( 'NONE', *, *, #7179, .T. ) ;
#3730 = CARTESIAN_POINT ( 'NONE',  ( 55.99999999999989342, 549.5810598491746077, -513.4200196135282113 ) ) ;
#3731 = DIRECTION ( 'NONE',  ( 0.000000000000000000, 0.09950371902099770793, -0.9950371902099891530 ) ) ;
#3732 = EDGE_CURVE ( 'NONE', #9656, #4133, #13570, .T. ) ;
#3733 = EDGE_CURVE ( 'NONE', #15480, #5615, #3409, .T. ) ;
#3734 = ADVANCED_FACE ( 'NONE', ( #4275 ), #2800, .F. ) ;
#3735 = LINE ( 'NONE', #6202, #12324 ) ;
#3736 = ADVANCED_FACE ( 'NONE', ( #13294 ), #6821, .F. ) ;
#3737 = DIRECTION ( 'NONE',  ( 0.000000000000000000, 0.000000000000000000, -1.000000000000000000 ) ) ;
#3738 = VERTEX_POINT ( 'NONE', #13032 ) ;
#3739 = CARTESIAN_POINT ( 'NONE',  ( 2.999999999999996891, 60.00000000000000711, 9.013878188659974811 ) ) ;
#3740 = CARTESIAN_POINT ( 'NONE',  ( -5.000000000000000000, 0.000000000000000000, 0.000000000000000000 ) ) ;
#3741 = ORIENTED_EDGE ( 'NONE', *, *, #9634, .T. ) ;
#3742 = AXIS2_PLACEMENT_3D ( 'NONE', #2218, #15109, #8595 ) ;
#3743 = AXIS2_PLACEMENT_3D ( 'NONE', #3349, #8424, #8675 ) ;
#3744 = DIRECTION ( 'NONE',  ( -1.000000000000000000, -0.000000000000000000, -0.000000000000000000 ) ) ;
#3745 = VERTEX_POINT ( 'NONE', #7945 ) ;
#3746 = CARTESIAN_POINT ( 'NONE',  ( 5.569974746830579804, 0.000000000000000000, 0.000000000000000000 ) ) ;
#3747 = ORIENTED_EDGE ( 'NONE', *, *, #15007, .F. ) ;
#3748 = VERTEX_POINT ( 'NONE', #6649 ) ;
#3749 = CARTESIAN_POINT ( 'NONE',  ( -26.00000000000002842, 3.000000000000000000, -39.99999999999999289 ) ) ;
#3750 = DIRECTION ( 'NONE',  ( -1.000000000000000000, -0.000000000000000000, -0.000000000000000000 ) ) ;
#3751 = DIRECTION ( 'NONE',  ( -0.8502651466878615727, 0.5263546146162958461, 0.000000000000000000 ) ) ;
#3752 = VECTOR ( 'NONE', #7519, 1000.000000000000000 ) ;
#3753 = ORIENTED_EDGE ( 'NONE', *, *, #10058, .T. ) ;
#3754 = CIRCLE ( 'NONE', #10331, 5.000000000000000888 ) ;
#3755 = DIRECTION ( 'NONE',  ( 0.000000000000000000, 0.000000000000000000, -1.000000000000000000 ) ) ;
#3756 = EDGE_CURVE ( 'NONE', #4921, #12044, #5542, .T. ) ;
#3757 = ADVANCED_FACE ( 'NONE', ( #14489 ), #5190, .T. ) ;
#3758 = VERTEX_POINT ( 'NONE', #2713 ) ;
#3759 = DIRECTION ( 'NONE',  ( 0.000000000000000000, 0.000000000000000000, -1.000000000000000000 ) ) ;
#3760 = EDGE_CURVE ( 'NONE', #11607, #3951, #13004, .T. ) ;
#3761 = DIRECTION ( 'NONE',  ( 1.000000000000000000, 0.000000000000000000, -0.000000000000000000 ) ) ;
#3762 = DIRECTION ( 'NONE',  ( 0.000000000000000000, 0.000000000000000000, 1.000000000000000000 ) ) ;
#3763 = CYLINDRICAL_SURFACE ( 'NONE', #16568, 13.69540538389601991 ) ;
#3764 = FACE_OUTER_BOUND ( 'NONE', #5292, .T. ) ;
#3765 = EDGE_LOOP ( 'NONE', ( #10611, #9542, #10668, #10333 ) ) ;
#3766 = AXIS2_PLACEMENT_3D ( 'NONE', #10617, #14569, #13460 ) ;
#3767 = DIRECTION ( 'NONE',  ( 0.000000000000000000, 1.000000000000000000, 0.000000000000000000 ) ) ;
#3768 = CARTESIAN_POINT ( 'NONE',  ( -19.00000000000001776, 8.000000000000000000, 40.00000000000000711 ) ) ;
#3769 = CARTESIAN_POINT ( 'NONE',  ( 22.99999999999998224, 10.00000000000000000, 37.00000000000000711 ) ) ;
#3770 = ORIENTED_EDGE ( 'NONE', *, *, #2973, .F. ) ;
#3771 = LINE ( 'NONE', #9010, #16256 ) ;
#3772 = AXIS2_PLACEMENT_3D ( 'NONE', #2649, #12874, #1363 ) ;
#3773 = CARTESIAN_POINT ( 'NONE',  ( -3.270000000000000462, 264.4632308570090231, 287.5298983642207986 ) ) ;
#3774 = ORIENTED_EDGE ( 'NONE', *, *, #5502, .T. ) ;
#3775 = DIRECTION ( 'NONE',  ( 1.000000000000000000, 0.000000000000000000, 0.000000000000000000 ) ) ;
#3776 = DIRECTION ( 'NONE',  ( 0.000000000000000000, 1.000000000000000000, 0.000000000000000000 ) ) ;
#3777 = CARTESIAN_POINT ( 'NONE',  ( -3.000000000000003109, 60.00000000000000711, 9.013878188659973034 ) ) ;
#3778 = EDGE_LOOP ( 'NONE', ( #15568, #15227, #2541, #10921 ) ) ;
#3779 = CARTESIAN_POINT ( 'NONE',  ( 0.000000000000000000, 620.7506394335853201, 0.000000000000000000 ) ) ;
#3780 = DIRECTION ( 'NONE',  ( 0.000000000000000000, 0.000000000000000000, 1.000000000000000000 ) ) ;
#3781 = CARTESIAN_POINT ( 'NONE',  ( 4.549999999999999822, 0.000000000000000000, 0.000000000000000000 ) ) ;
#3782 = EDGE_LOOP ( 'NONE', ( #15943, #8785, #15454, #12833 ) ) ;
#3783 = CARTESIAN_POINT ( 'NONE',  ( 36.99999999999999289, 10.00000000000000000, -22.99999999999999645 ) ) ;
#3784 = AXIS2_PLACEMENT_3D ( 'NONE', #767, #15271, #14063 ) ;
#3785 = ADVANCED_FACE ( 'NONE', ( #9590 ), #5637, .F. ) ;
#3786 = VERTEX_POINT ( 'NONE', #3313 ) ;
#3787 = DIRECTION ( 'NONE',  ( -0.000000000000000000, -1.000000000000000000, -0.000000000000000000 ) ) ;
#3788 = LINE ( 'NONE', #9027, #3158 ) ;
#3789 = ADVANCED_FACE ( 'NONE', ( #12415 ), #12259, .T. ) ;
#3790 = CARTESIAN_POINT ( 'NONE',  ( 37.00000000000000000, 68.00000000000000000, 23.00000000000001066 ) ) ;
#3791 = ORIENTED_EDGE ( 'NONE', *, *, #10955, .T. ) ;
#3792 = DIRECTION ( 'NONE',  ( 0.000000000000000000, 0.000000000000000000, -1.000000000000000000 ) ) ;
#3793 = CARTESIAN_POINT ( 'NONE',  ( -33.99999999999997158, 0.000000000000000000, -25.99999999999999645 ) ) ;
#3794 = ORIENTED_EDGE ( 'NONE', *, *, #12603, .T. ) ;
#3795 = VECTOR ( 'NONE', #100, 1000.000000000000114 ) ;
#3796 = CARTESIAN_POINT ( 'NONE',  ( -46.99999999999988631, 559.9933750504617365, -546.7230258972048205 ) ) ;
#3797 = ORIENTED_EDGE ( 'NONE', *, *, #7342, .F. ) ;
#3798 = ORIENTED_EDGE ( 'NONE', *, *, #4009, .T. ) ;
#3799 = DIRECTION ( 'NONE',  ( 1.000000000000000000, -0.000000000000000000, 0.000000000000000000 ) ) ;
#3800 = ORIENTED_EDGE ( 'NONE', *, *, #3726, .F. ) ;
#3801 = DIRECTION ( 'NONE',  ( -0.5444686587298510627, 0.8387811869974892698, 0.000000000000000000 ) ) ;
#3802 = EDGE_LOOP ( 'NONE', ( #423, #10749, #16222, #4761 ) ) ;
#3803 = EDGE_CURVE ( 'NONE', #9900, #2103, #745, .T. ) ;
#3804 = ORIENTED_EDGE ( 'NONE', *, *, #5179, .T. ) ;
#3805 = AXIS2_PLACEMENT_3D ( 'NONE', #5922, #7287, #3352 ) ;
#3806 = CARTESIAN_POINT ( 'NONE',  ( 25.99999999999999645, 68.00000000000000000, 40.00000000000002132 ) ) ;
#3807 = DIRECTION ( 'NONE',  ( -1.000000000000000000, 0.000000000000000000, -0.000000000000000000 ) ) ;
#3808 = ORIENTED_EDGE ( 'NONE', *, *, #12141, .F. ) ;
#3809 = LINE ( 'NONE', #11706, #9973 ) ;
#3810 = CARTESIAN_POINT ( 'NONE',  ( 6.299999999999999822, 18.50000000000000000, 0.000000000000000000 ) ) ;
#3811 = VERTEX_POINT ( 'NONE', #13637 ) ;
#3812 = CARTESIAN_POINT ( 'NONE',  ( -23.00000000000002132, 10.00000000000000000, 37.00000000000000711 ) ) ;
#3813 = CARTESIAN_POINT ( 'NONE',  ( -23.00000000000003197, 0.000000000000000000, 34.00000000000000711 ) ) ;
#3814 = VERTEX_POINT ( 'NONE', #14750 ) ;
#3815 = ADVANCED_FACE ( 'NONE', ( #4357 ), #11209, .F. ) ;
#3816 = FACE_OUTER_BOUND ( 'NONE', #5430, .T. ) ;
#3817 = ORIENTED_EDGE ( 'NONE', *, *, #521, .F. ) ;
#3818 = CYLINDRICAL_SURFACE ( 'NONE', #3725, 35.00000000000000711 ) ;
#3819 = ORIENTED_EDGE ( 'NONE', *, *, #9144, .F. ) ;
#3820 = ADVANCED_FACE ( 'NONE', ( #13549 ), #8471, .T. ) ;
#3821 = AXIS2_PLACEMENT_3D ( 'NONE', #16556, #9794, #1959 ) ;
#3822 = ORIENTED_EDGE ( 'NONE', *, *, #9415, .F. ) ;
#3823 = FACE_OUTER_BOUND ( 'NONE', #15174, .T. ) ;
#3824 = DIRECTION ( 'NONE',  ( 0.000000000000000000, 0.000000000000000000, -1.000000000000000000 ) ) ;
#3825 = DIRECTION ( 'NONE',  ( 0.000000000000000000, 0.000000000000000000, 1.000000000000000000 ) ) ;
#3826 = ORIENTED_EDGE ( 'NONE', *, *, #373, .T. ) ;
#3827 = DIRECTION ( 'NONE',  ( -1.000000000000000000, -0.000000000000000000, -0.000000000000000000 ) ) ;
#3828 = PRODUCT_DEFINITION_SHAPE ( 'NONE', 'NONE',  #6603 ) ;
#3829 = CARTESIAN_POINT ( 'NONE',  ( 46.99999999999988631, 523.2161522479888163, -516.5890438806160319 ) ) ;
#3830 = DIRECTION ( 'NONE',  ( -1.156482317317875275E-15, 0.000000000000000000, -1.000000000000000000 ) ) ;
#3831 = CARTESIAN_POINT ( 'NONE',  ( 394.0000000000001137, 234.3157724647196289, -17.15546574335979813 ) ) ;
#3832 = FACE_OUTER_BOUND ( 'NONE', #7425, .T. ) ;
#3833 = AXIS2_PLACEMENT_3D ( 'NONE', #10701, #5373, #1684 ) ;
#3834 = EDGE_CURVE ( 'NONE', #7927, #8784, #8058, .T. ) ;
#3835 = LINE ( 'NONE', #9073, #11640 ) ;
#3836 = DIRECTION ( 'NONE',  ( 0.000000000000000000, 0.000000000000000000, -1.000000000000000000 ) ) ;
#3838 = ORIENTED_EDGE ( 'NONE', *, *, #8551, .F. ) ;
#3837 = ORIENTED_EDGE ( 'NONE', *, *, #10570, .T. ) ;
#3839 = LINE ( 'NONE', #14158, #13031 ) ;
#3840 =( GEOMETRIC_REPRESENTATION_CONTEXT ( 3 ) GLOBAL_UNCERTAINTY_ASSIGNED_CONTEXT ( ( #10648 ) ) GLOBAL_UNIT_ASSIGNED_CONTEXT ( ( #7623, #16729, #2394 ) ) REPRESENTATION_CONTEXT ( 'NONE', 'WORKASPACE' ) );
#3841 = EDGE_CURVE ( 'NONE', #14813, #9616, #8394, .T. ) ;
#3842 = EDGE_CURVE ( 'NONE', #10263, #2977, #13464, .T. ) ;
#3843 = EDGE_CURVE ( 'NONE', #219, #4052, #1934, .T. ) ;
#3844 = DIRECTION ( 'NONE',  ( 0.000000000000000000, 0.000000000000000000, 1.000000000000000000 ) ) ;
#3845 = EDGE_CURVE ( 'NONE', #14012, #12430, #6910, .T. ) ;
#3846 = CARTESIAN_POINT ( 'NONE',  ( 0.000000000000000000, 339.4485271457185718, -110.7359021160857537 ) ) ;
#3847 = VECTOR ( 'NONE', #2323, 1000.000000000000000 ) ;
#3848 = EDGE_LOOP ( 'NONE', ( #2770, #9341, #11773, #16373, #1649, #11112, #13691, #8113, #705, #11323, #13035, #3217, #13153, #15971, #14260, #2801 ) ) ;
#3849 = VECTOR ( 'NONE', #675, 1000.000000000000000 ) ;
#3850 = FACE_OUTER_BOUND ( 'NONE', #3852, .T. ) ;
#3851 = DIRECTION ( 'NONE',  ( -0.000000000000000000, 2.220446049250308742E-15, 1.000000000000000000 ) ) ;
#3852 = EDGE_LOOP ( 'NONE', ( #6001, #10937, #9903, #3866 ) ) ;
#3853 = DIRECTION ( 'NONE',  ( 0.000000000000000000, 1.000000000000000000, 0.000000000000000000 ) ) ;
#3854 = CARTESIAN_POINT ( 'NONE',  ( -31.00000000000003553, 19.00000000000000000, -21.00000000000000000 ) ) ;
#3855 = DIRECTION ( 'NONE',  ( 0.000000000000000000, 1.000000000000000000, 0.000000000000000000 ) ) ;
#3856 = EDGE_LOOP ( 'NONE', ( #2844, #11359, #12646, #16149 ) ) ;
#3857 = FACE_OUTER_BOUND ( 'NONE', #4618, .T. ) ;
#3858 = CARTESIAN_POINT ( 'NONE',  ( 10.00000000000000000, 309.2289037985890445, -146.8198051533984199 ) ) ;
#3859 = CARTESIAN_POINT ( 'NONE',  ( 31.00000000000000711, 0.000000000000000000, -30.99999999999999289 ) ) ;
#3860 = VERTEX_POINT ( 'NONE', #10880 ) ;
#3861 = VECTOR ( 'NONE', #2359, 1000.000000000000000 ) ;
#3862 = FACE_OUTER_BOUND ( 'NONE', #10803, .T. ) ;
#3863 = ITEM_DEFINED_TRANSFORMATION ( 'NONE', 'NONE', #13574,  #1488 ) ;
#3864 = ADVANCED_FACE ( 'NONE', ( #654 ), #12170, .T. ) ;
#3865 = DIRECTION ( 'NONE',  ( -0.000000000000000000, 1.000000000000000000, -0.000000000000000000 ) ) ;
#3866 = ORIENTED_EDGE ( 'NONE', *, *, #2606, .T. ) ;
#3867 = CARTESIAN_POINT ( 'NONE',  ( -40.00000000000000711, 0.000000000000000000, 26.00000000000000000 ) ) ;
#3868 = FACE_OUTER_BOUND ( 'NONE', #11774, .T. ) ;
#3869 = AXIS2_PLACEMENT_3D ( 'NONE', #16536, #4678, #4771 ) ;
#3870 = DIRECTION ( 'NONE',  ( 0.000000000000000000, 0.000000000000000000, -1.000000000000000000 ) ) ;
#3871 = ORIENTED_EDGE ( 'NONE', *, *, #15156, .T. ) ;
#3872 = DIRECTION ( 'NONE',  ( 0.000000000000000000, 0.000000000000000000, 1.000000000000000000 ) ) ;
#3873 = FACE_OUTER_BOUND ( 'NONE', #4063, .T. ) ;
#3874 = VERTEX_POINT ( 'NONE', #5718 ) ;
#3875 = DIRECTION ( 'NONE',  ( 0.000000000000000000, 0.000000000000000000, 1.000000000000000000 ) ) ;
#3876 = EDGE_CURVE ( 'NONE', #1572, #1879, #16195, .T. ) ;
#3877 = EDGE_LOOP ( 'NONE', ( #14895, #16664, #860, #525, #223, #2310, #9842, #4123, #13755, #4650, #6633, #3564, #5613, #12900, #14405, #7566, #8689, #16252, #9513, #9757, #11383, #13609, #11213, #4484, #16267, #1864, #13880, #7192 ) ) ;
#3878 = ORIENTED_EDGE ( 'NONE', *, *, #13612, .F. ) ;
#3879 = DIRECTION ( 'NONE',  ( -0.000000000000000000, -1.000000000000000000, -0.000000000000000000 ) ) ;
#3880 = VERTEX_POINT ( 'NONE', #14913 ) ;
#3881 = CARTESIAN_POINT ( 'NONE',  ( 3.270000000000000462, -3.240394488364190195, -37.52989836422090519 ) ) ;
#3882 = VECTOR ( 'NONE', #8384, 1000.000000000000114 ) ;
#3883 = ORIENTED_EDGE ( 'NONE', *, *, #10148, .T. ) ;
#3884 = EDGE_LOOP ( 'NONE', ( #7231, #1643, #11519, #4340 ) ) ;
#3885 = AXIS2_PLACEMENT_3D ( 'NONE', #2911, #9530, #10636 ) ;
#3886 = AXIS2_PLACEMENT_3D ( 'NONE', #8478, #13881, #2192 ) ;
#3887 = CARTESIAN_POINT ( 'NONE',  ( 394.0000000000001137, 339.1725919290084335, -104.9456657433597968 ) ) ;
#3888 = CYLINDRICAL_SURFACE ( 'NONE', #14934, 18.49999999999998934 ) ;
#3889 = ORIENTED_EDGE ( 'NONE', *, *, #6847, .F. ) ;
#3890 = DIRECTION ( 'NONE',  ( 1.000000000000000000, -0.000000000000000000, -0.000000000000000000 ) ) ;
#3891 = DIRECTION ( 'NONE',  ( 0.000000000000000000, 0.000000000000000000, -1.000000000000000000 ) ) ;
#3892 = PLANE ( 'NONE',  #4843 ) ;
#3893 = CIRCLE ( 'NONE', #3068, 3.299999999999997158 ) ;
#3894 = DIRECTION ( 'NONE',  ( 1.000000000000000000, 0.000000000000000000, 0.000000000000000000 ) ) ;
#3895 = ORIENTED_EDGE ( 'NONE', *, *, #540, .T. ) ;
#3896 = CARTESIAN_POINT ( 'NONE',  ( -440.0000000000000568, 425.7506394335853201, 109.9999999999999858 ) ) ;
#3897 = CARTESIAN_POINT ( 'NONE',  ( 10.00000000000000000, 435.2933666400819561, -575.6295912558023247 ) ) ;
#3898 = ORIENTED_EDGE ( 'NONE', *, *, #15895, .F. ) ;
#3899 = CIRCLE ( 'NONE', #5808, 9.000000000000007105 ) ;
#3900 = AXIS2_PLACEMENT_3D ( 'NONE', #3254, #7349, #12598 ) ;
#3901 = VECTOR ( 'NONE', #12321, 1000.000000000000000 ) ;
#3902 = LINE ( 'NONE', #8898, #4670 ) ;
#3903 = VERTEX_POINT ( 'NONE', #11043 ) ;
#3904 = CARTESIAN_POINT ( 'NONE',  ( 30.99999999999997513, 10.00000000000000000, 25.99999999999999645 ) ) ;
#3905 = ORIENTED_EDGE ( 'NONE', *, *, #13504, .F. ) ;
#3906 = APPLICATION_CONTEXT ( 'automotive_design' ) ;
#3907 = AXIS2_PLACEMENT_3D ( 'NONE', #16665, #11681, #12885 ) ;
#3908 = ORIENTED_EDGE ( 'NONE', *, *, #10151, .T. ) ;
#3909 = DIRECTION ( 'NONE',  ( 0.000000000000000000, 1.000000000000000000, -0.000000000000000000 ) ) ;
#3910 = DIRECTION ( 'NONE',  ( 1.000000000000000000, -0.000000000000000000, 0.000000000000000000 ) ) ;
#3911 = LINE ( 'NONE', #9063, #5850 ) ;
#3912 = ORIENTED_EDGE ( 'NONE', *, *, #12768, .T. ) ;
#3913 = EDGE_CURVE ( 'NONE', #11935, #14137, #5799, .T. ) ;
#3914 = LINE ( 'NONE', #14396, #6903 ) ;
#3915 = VECTOR ( 'NONE', #7529, 1000.000000000000000 ) ;
#3916 = CARTESIAN_POINT ( 'NONE',  ( 0.000000000000000000, 10.00000000000000000, -9.500000000000000000 ) ) ;
#3917 = B_SPLINE_CURVE_WITH_KNOTS ( 'NONE', 3,
 ( #5962, #13544, #1776, #6995, #12327, #16438, #12253, #489, #10956, #14908 ),
 .UNSPECIFIED., .F., .F.,
 ( 4, 2, 2, 2, 4 ),
 ( 0.000000000000000000, 0.2500000000000000000, 0.5000000000000000000, 0.7500000000000000000, 1.000000000000000000 ),
 .UNSPECIFIED. ) ;
#3918 = CARTESIAN_POINT ( 'NONE',  ( 26.00000000000000711, 68.00000000000000000, -31.00000000000002487 ) ) ;
#3919 = CARTESIAN_POINT ( 'NONE',  ( 0.03302700000138451830, 193.3948361422361870, 37.50583589681554741 ) ) ;
#3920 = CYLINDRICAL_SURFACE ( 'NONE', #4712, 3.300000000000000711 ) ;
#3921 = VECTOR ( 'NONE', #7190, 1000.000000000000000 ) ;
#3922 = EDGE_CURVE ( 'NONE', #9423, #5597, #14923, .T. ) ;
#3923 = CYLINDRICAL_SURFACE ( 'NONE', #9171, 13.69540538389601991 ) ;
#3924 = CARTESIAN_POINT ( 'NONE',  ( 2.625000000000000000, 0.000000000000000000, 0.000000000000000000 ) ) ;
#3926 = VERTEX_POINT ( 'NONE', #16367 ) ;
#3925 = ORIENTED_EDGE ( 'NONE', *, *, #16935, .T. ) ;
#3927 = DIRECTION ( 'NONE',  ( -0.000000000000000000, 1.000000000000000000, -1.224646799147353207E-16 ) ) ;
#3928 = AXIS2_PLACEMENT_3D ( 'NONE', #6206, #15502, #14134 ) ;
#3929 = AXIS2_PLACEMENT_3D ( 'NONE', #16041, #13305, #5461 ) ;
#3930 = DIRECTION ( 'NONE',  ( 0.000000000000000000, 0.000000000000000000, 1.000000000000000000 ) ) ;
#3931 = DIRECTION ( 'NONE',  ( -1.000000000000000000, -0.000000000000000000, -0.000000000000000000 ) ) ;
#3932 = DIRECTION ( 'NONE',  ( 0.000000000000000000, 0.000000000000000000, 1.000000000000000000 ) ) ;
#3933 = AXIS2_PLACEMENT_3D ( 'NONE', #12306, #8361, #11969 ) ;
#3934 = ORIENTED_EDGE ( 'NONE', *, *, #3404, .F. ) ;
#3935 = EDGE_CURVE ( 'NONE', #13578, #851, #7490, .T. ) ;
#3936 = DIRECTION ( 'NONE',  ( -0.000000000000000000, -1.000000000000000000, 0.000000000000000000 ) ) ;
#3937 = VECTOR ( 'NONE', #7136, 1000.000000000000000 ) ;
#3938 = AXIS2_PLACEMENT_3D ( 'NONE', #14993, #11370, #16606 ) ;
#3939 = CARTESIAN_POINT ( 'NONE',  ( -35.00000000000000000, 8.000000000000000000, 20.99999999999999289 ) ) ;
#3940 = EDGE_LOOP ( 'NONE', ( #3073, #16399, #7334, #7666 ) ) ;
#3941 = CARTESIAN_POINT ( 'NONE',  ( -45.00000000000000000, 515.4878487013597805, -521.7230258972047068 ) ) ;
#3942 = VECTOR ( 'NONE', #7402, 1000.000000000000000 ) ;
#3943 = EDGE_CURVE ( 'NONE', #14523, #6600, #11901, .T. ) ;
#3944 = DIRECTION ( 'NONE',  ( -1.000000000000000000, -0.000000000000000000, -0.000000000000000000 ) ) ;
#3945 = DIRECTION ( 'NONE',  ( -0.000000000000000000, -1.000000000000000000, -0.000000000000000000 ) ) ;
#3946 = EDGE_CURVE ( 'NONE', #2956, #2142, #10327, .T. ) ;
#3947 = ADVANCED_FACE ( 'NONE', ( #8953 ), #12897, .F. ) ;
#3948 = DIRECTION ( 'NONE',  ( -1.196361017915039486E-16, -0.000000000000000000, -1.000000000000000000 ) ) ;
#3949 = CARTESIAN_POINT ( 'NONE',  ( -46.99999999999988631, 473.6663340069158039, -561.9448123979092315 ) ) ;
#3950 = CARTESIAN_POINT ( 'NONE',  ( 0.000000000000000000, 451.4647406485092915, -149.8062676851188257 ) ) ;
#3951 = VERTEX_POINT ( 'NONE', #11521 ) ;
#3952 = VECTOR ( 'NONE', #8522, 1000.000000000000000 ) ;
#3953 = DIRECTION ( 'NONE',  ( 1.000000000000000000, 0.000000000000000000, 0.000000000000000000 ) ) ;
#3954 = ITEM_DEFINED_TRANSFORMATION ( 'NONE', 'NONE', #15214,  #1488 ) ;
#3955 = STYLED_ITEM ( 'NONE', ( #9638 ), #3094 ) ;
#3956 =( NAMED_UNIT ( * ) SI_UNIT ( $, .STERADIAN. ) SOLID_ANGLE_UNIT ( ) );
#3957 = VECTOR ( 'NONE', #10146, 1000.000000000000000 ) ;
#3958 = CARTESIAN_POINT ( 'NONE',  ( -34.99999999999998579, -20.00000000000000000, 21.00000000000000355 ) ) ;
#3959 = ORIENTED_EDGE ( 'NONE', *, *, #11735, .F. ) ;
#3960 = VECTOR ( 'NONE', #15525, 1000.000000000000000 ) ;
#3961 = DIRECTION ( 'NONE',  ( -1.000000000000000000, -0.000000000000000000, -0.000000000000000000 ) ) ;
#3962 = CARTESIAN_POINT ( 'NONE',  ( 0.000000000000000000, 0.000000000000000000, 22.50000000000000000 ) ) ;
#3963 = TOROIDAL_SURFACE ( 'NONE', #14660, 4.695405383895982609, 9.000000000000000000 ) ;
#3964 = CARTESIAN_POINT ( 'NONE',  ( -40.00000000000000711, 8.000000000000000000, -19.00000000000000355 ) ) ;
#3965 = EDGE_LOOP ( 'NONE', ( #8553, #2831, #1656, #3970 ) ) ;
#3966 = CARTESIAN_POINT ( 'NONE',  ( 19.99999999999995381, 0.000000000000000000, -36.99999999999999289 ) ) ;
#3967 = EDGE_CURVE ( 'NONE', #9064, #7586, #2413, .T. ) ;
#3968 = DIRECTION ( 'NONE',  ( 0.000000000000000000, -0.9848077530122090195, 0.1736481776669249744 ) ) ;
#3969 = DIRECTION ( 'NONE',  ( 0.000000000000000000, 0.000000000000000000, -1.000000000000000000 ) ) ;
#3970 = ORIENTED_EDGE ( 'NONE', *, *, #663, .T. ) ;
#3971 = EDGE_CURVE ( 'NONE', #16075, #6598, #15565, .T. ) ;
#3972 =( GEOMETRIC_REPRESENTATION_CONTEXT ( 3 ) GLOBAL_UNCERTAINTY_ASSIGNED_CONTEXT ( ( #13971 ) ) GLOBAL_UNIT_ASSIGNED_CONTEXT ( ( #11114, #9830, #10080 ) ) REPRESENTATION_CONTEXT ( 'NONE', 'WORKASPACE' ) );
#3973 = ADVANCED_FACE ( 'NONE', ( #7903 ), #108, .T. ) ;
#3974 = DIRECTION ( 'NONE',  ( 0.000000000000000000, 0.000000000000000000, -1.000000000000000000 ) ) ;
#3975 = ORIENTED_EDGE ( 'NONE', *, *, #3404, .T. ) ;
#3976 = ORIENTED_EDGE ( 'NONE', *, *, #4061, .T. ) ;
#3977 = CARTESIAN_POINT ( 'NONE',  ( 55.99999999999989342, 559.9933750504617365, -560.4184312811007658 ) ) ;
#3978 = AXIS2_PLACEMENT_3D ( 'NONE', #16733, #4893, #9021 ) ;
#3979 = EDGE_LOOP ( 'NONE', ( #2599, #12838, #10560, #11598 ) ) ;
#3980 = ORIENTED_EDGE ( 'NONE', *, *, #9582, .F. ) ;
#3981 = DIRECTION ( 'NONE',  ( 0.000000000000000000, 0.000000000000000000, 1.000000000000000000 ) ) ;
#3982 = EDGE_LOOP ( 'NONE', ( #13146, #5828, #1714, #7225 ) ) ;
#3983 = ORIENTED_EDGE ( 'NONE', *, *, #10885, .T. ) ;
#3984 = PRODUCT_DEFINITION_FORMATION_WITH_SPECIFIED_SOURCE ( 'ANY', '', #8762, .NOT_KNOWN. ) ;
#3985 = DIRECTION ( 'NONE',  ( 0.000000000000000000, 0.000000000000000000, -1.000000000000000000 ) ) ;
#3986 = FACE_OUTER_BOUND ( 'NONE', #16369, .T. ) ;
#3987 = VERTEX_POINT ( 'NONE', #1052 ) ;
#3988 = AXIS2_PLACEMENT_3D ( 'NONE', #5475, #13223, #1708 ) ;
#3989 = CARTESIAN_POINT ( 'NONE',  ( -31.00000000000005329, 10.00000000000000000, -26.00000000000000355 ) ) ;
#3990 = DIRECTION ( 'NONE',  ( 0.000000000000000000, 0.000000000000000000, 1.000000000000000000 ) ) ;
#3991 = CARTESIAN_POINT ( 'NONE',  ( 6.649999999999999467, 0.000000000000000000, 0.000000000000000000 ) ) ;
#3992 = ORIENTED_EDGE ( 'NONE', *, *, #11613, .T. ) ;
#3993 = DIRECTION ( 'NONE',  ( 0.000000000000000000, 0.000000000000000000, 1.000000000000000000 ) ) ;
#3994 = CYLINDRICAL_SURFACE ( 'NONE', #15450, 8.000000000000000000 ) ;
#3995 = ORIENTED_EDGE ( 'NONE', *, *, #714, .F. ) ;
#3996 = CARTESIAN_POINT ( 'NONE',  ( 0.000000000000000000, 0.000000000000000000, 0.000000000000000000 ) ) ;
#3997 = EDGE_LOOP ( 'NONE', ( #12000, #5163 ) ) ;
#3998 = CARTESIAN_POINT ( 'NONE',  ( -32.00000000000000711, 10.00000000000000000, -23.00000000000000000 ) ) ;
#3999 = CIRCLE ( 'NONE', #7814, 4.695405383896011919 ) ;
#4000 = ORIENTED_EDGE ( 'NONE', *, *, #1942, .F. ) ;
#4001 = VERTEX_POINT ( 'NONE', #16755 ) ;
#4002 = DIRECTION ( 'NONE',  ( -1.000000000000000000, -0.000000000000000000, -0.000000000000000000 ) ) ;
#4003 = EDGE_CURVE ( 'NONE', #2412, #2603, #3719, .T. ) ;
#4004 = CARTESIAN_POINT ( 'NONE',  ( -20.99999999999999645, 8.000000000000000000, -35.00000000000000711 ) ) ;
#4005 = CARTESIAN_POINT ( 'NONE',  ( -23.00000000000002132, 10.00000000000000000, 31.00000000000003553 ) ) ;
#4006 = VERTEX_POINT ( 'NONE', #11604 ) ;
#4007 = CYLINDRICAL_SURFACE ( 'NONE', #1151, 187.4999999999998863 ) ;
#4008 = LINE ( 'NONE', #4936, #10516 ) ;
#4009 = EDGE_CURVE ( 'NONE', #7947, #2523, #15640, .T. ) ;
#4010 = DIRECTION ( 'NONE',  ( -0.000000000000000000, -1.000000000000000000, 0.000000000000000000 ) ) ;
#4011 = LINE ( 'NONE', #13289, #1851 ) ;
#4012 = CARTESIAN_POINT ( 'NONE',  ( 37.50000000000000000, 196.3050121726289206, 0.000000000000000000 ) ) ;
#4013 = DIRECTION ( 'NONE',  ( 0.000000000000000000, 0.000000000000000000, -1.000000000000000000 ) ) ;
#4014 = CYLINDRICAL_SURFACE ( 'NONE', #5704, 14.59999999999999964 ) ;
#4016 = ORIENTED_EDGE ( 'NONE', *, *, #13904, .T. ) ;
#4015 = ORIENTED_EDGE ( 'NONE', *, *, #8829, .T. ) ;
#4017 = CARTESIAN_POINT ( 'NONE',  ( 4.163799117101000559E-15, 23.00000000000000000, 34.00000000000000000 ) ) ;
#4018 = PRODUCT_DEFINITION ( 'UNKNOWN', '', #4254, #9300 ) ;
#4019 = VECTOR ( 'NONE', #15866, 1000.000000000000000 ) ;
#4020 = CARTESIAN_POINT ( 'NONE',  ( 0.7365999999999761627, 286.2094592450220034, 37.20452120302228138 ) ) ;
#4021 = VECTOR ( 'NONE', #1187, 1000.000000000000000 ) ;
#4022 = DIRECTION ( 'NONE',  ( -0.000000000000000000, -0.000000000000000000, 1.000000000000000000 ) ) ;
#4023 = LINE ( 'NONE', #12213, #10770 ) ;
#4024 = ADVANCED_FACE ( 'NONE', ( #9924 ), #14274, .F. ) ;
#4025 = ORIENTED_EDGE ( 'NONE', *, *, #3477, .F. ) ;
#4026 = CARTESIAN_POINT ( 'NONE',  ( -3.270000000000000018, 220.1329686874181562, 287.5298983642209123 ) ) ;
#4027 = CARTESIAN_POINT ( 'NONE',  ( 46.99999999999988631, 473.6663340069158039, -557.2494070140132862 ) ) ;
#4028 = ORIENTED_EDGE ( 'NONE', *, *, #9160, .F. ) ;
#4029 = LINE ( 'NONE', #9266, #15091 ) ;
#4030 = DIRECTION ( 'NONE',  ( -0.000000000000000000, -0.000000000000000000, 1.000000000000000000 ) ) ;
#4031 = ORIENTED_EDGE ( 'NONE', *, *, #5992, .F. ) ;
#4032 = CARTESIAN_POINT ( 'NONE',  ( -31.00000000000000000, 11.00000000000000000, 25.99999999999999645 ) ) ;
#4033 = CYLINDRICAL_SURFACE ( 'NONE', #9263, 12.50000000000001066 ) ;
#4034 = CARTESIAN_POINT ( 'NONE',  ( -8.881784197001250351E-16, -17.85000000000000142, 2.225795557450314789E-15 ) ) ;
#4035 = ORIENTED_EDGE ( 'NONE', *, *, #14351, .F. ) ;
#4036 = DIRECTION ( 'NONE',  ( 1.000000000000000000, -0.000000000000000000, -0.000000000000000000 ) ) ;
#4037 = EDGE_CURVE ( 'NONE', #13742, #10036, #6267, .T. ) ;
#4038 = DIRECTION ( 'NONE',  ( 0.000000000000000000, 0.000000000000000000, -1.000000000000000000 ) ) ;
#4039 = AXIS2_PLACEMENT_3D ( 'NONE', #6040, #16442, #4668 ) ;
#4040 = EDGE_CURVE ( 'NONE', #15, #15508, #15157, .T. ) ;
#4041 = ORIENTED_EDGE ( 'NONE', *, *, #5442, .F. ) ;
#4042 = ADVANCED_FACE ( 'NONE', ( #6521 ), #17, .T. ) ;
#4043 = CARTESIAN_POINT ( 'NONE',  ( 55.99999999999989342, 523.2161522479888163, -502.8936384967199729 ) ) ;
#4044 = CARTESIAN_POINT ( 'NONE',  ( 31.00000000000000000, 19.00000000000000000, -31.00000000000000355 ) ) ;
#4045 = CARTESIAN_POINT ( 'NONE',  ( 46.99999999999988631, 523.2161522479888163, -498.1982331128240276 ) ) ;
#4046 = ORIENTED_EDGE ( 'NONE', *, *, #3560, .F. ) ;
#4047 = CARTESIAN_POINT ( 'NONE',  ( 26.00000000000000000, 19.00000000000000000, 40.00000000000001421 ) ) ;
#4048 = FACE_OUTER_BOUND ( 'NONE', #6027, .T. ) ;
#4049 = DIRECTION ( 'NONE',  ( 0.000000000000000000, 0.000000000000000000, 1.000000000000000000 ) ) ;
#4050 = ORIENTED_EDGE ( 'NONE', *, *, #15398, .T. ) ;
#4051 = DIRECTION ( 'NONE',  ( 0.000000000000000000, -0.3746065934159093502, -0.9271838545667885345 ) ) ;
#4052 = VERTEX_POINT ( 'NONE', #10239 ) ;
#4053 = ORIENTED_EDGE ( 'NONE', *, *, #2185, .T. ) ;
#4054 = CIRCLE ( 'NONE', #13659, 3.300000000000025135 ) ;
#4055 = DIRECTION ( 'NONE',  ( -0.000000000000000000, -1.000000000000000000, -0.000000000000000000 ) ) ;
#4056 = ADVANCED_FACE ( 'NONE', ( #12819 ), #15482, .T. ) ;
#4057 = ORIENTED_EDGE ( 'NONE', *, *, #11829, .T. ) ;
#4058 = APPLICATION_PROTOCOL_DEFINITION ( 'draft international standard', 'automotive_design', 1998, #8297 ) ;
#4059 = ORIENTED_EDGE ( 'NONE', *, *, #2574, .F. ) ;
#4060 = EDGE_CURVE ( 'NONE', #7330, #9826, #12988, .T. ) ;
#4061 = EDGE_CURVE ( 'NONE', #14215, #3583, #15726, .T. ) ;
#4062 = EDGE_CURVE ( 'NONE', #11045, #12540, #14449, .T. ) ;
#4063 = EDGE_LOOP ( 'NONE', ( #12236, #5924, #16175, #9261 ) ) ;
#4064 = EDGE_CURVE ( 'NONE', #13088, #11305, #198, .T. ) ;
#4065 = CARTESIAN_POINT ( 'NONE',  ( -40.00000000000000000, 0.000000000000000000, 26.00000000000000355 ) ) ;
#4066 = PLANE ( 'NONE',  #13003 ) ;
#4067 = EDGE_LOOP ( 'NONE', ( #2715, #5750, #10092, #3084 ) ) ;
#4068 = LINE ( 'NONE', #5346, #11599 ) ;
#4069 = CIRCLE ( 'NONE', #789, 9.999999999999998224 ) ;
#4070 = CARTESIAN_POINT ( 'NONE',  ( 31.00000000000003553, 8.000000000000000000, 20.99999999999999289 ) ) ;
#4071 = VERTEX_POINT ( 'NONE', #6788 ) ;
#4072 = LINE ( 'NONE', #8269, #927 ) ;
#4073 = ORIENTED_EDGE ( 'NONE', *, *, #1837, .T. ) ;
#4074 = CARTESIAN_POINT ( 'NONE',  ( 45.00000000000000000, 493.2350855268092573, -585.2659423243250103 ) ) ;
#4075 = DIRECTION ( 'NONE',  ( -0.000000000000000000, -1.000000000000000000, -0.000000000000000000 ) ) ;
#4076 = VERTEX_POINT ( 'NONE', #9374 ) ;
#4077 = DIRECTION ( 'NONE',  ( -0.000000000000000000, 1.000000000000000000, -0.000000000000000000 ) ) ;
#4078 = ORIENTED_EDGE ( 'NONE', *, *, #1019, .F. ) ;
#4079 = DIRECTION ( 'NONE',  ( 0.000000000000000000, 0.000000000000000000, -1.000000000000000000 ) ) ;
#4080 = AXIS2_PLACEMENT_3D ( 'NONE', #12166, #4271, #9506 ) ;
#4081 = ORIENTED_EDGE ( 'NONE', *, *, #11376, .T. ) ;
#4082 = ORIENTED_EDGE ( 'NONE', *, *, #2455, .F. ) ;
#4083 = FACE_OUTER_BOUND ( 'NONE', #14220, .T. ) ;
#4084 = ADVANCED_FACE ( 'NONE', ( #16074 ), #4320, .T. ) ;
#4085 = DIRECTION ( 'NONE',  ( 0.000000000000000000, 0.000000000000000000, 1.000000000000000000 ) ) ;
#4086 = FACE_OUTER_BOUND ( 'NONE', #9998, .T. ) ;
#4087 = ORIENTED_EDGE ( 'NONE', *, *, #12760, .T. ) ;
#4088 = CARTESIAN_POINT ( 'NONE',  ( -37.00000000000000000, 68.00000000000000000, -22.99999999999999645 ) ) ;
#4089 = CARTESIAN_POINT ( 'NONE',  ( 25.99999999999996092, 3.000000000000000000, 31.00000000000004263 ) ) ;
#4090 = DIRECTION ( 'NONE',  ( 0.000000000000000000, 0.000000000000000000, -1.000000000000000000 ) ) ;
#4091 = CARTESIAN_POINT ( 'NONE',  ( 45.00000000000000000, 493.2350855268092573, -571.5705369404290650 ) ) ;
#4092 = CARTESIAN_POINT ( 'NONE',  ( 4.549999999999999822, 0.000000000000000000, 0.000000000000000000 ) ) ;
#4093 = PLANE ( 'NONE',  #16018 ) ;
#4094 = EDGE_CURVE ( 'NONE', #2740, #15912, #9453, .T. ) ;
#4096 = ORIENTED_EDGE ( 'NONE', *, *, #3118, .T. ) ;
#4095 = ORIENTED_EDGE ( 'NONE', *, *, #553, .T. ) ;
#4097 = LINE ( 'NONE', #5458, #12226 ) ;
#4098 = AXIS2_PLACEMENT_3D ( 'NONE', #2883, #15930, #4090 ) ;
#4099 = CARTESIAN_POINT ( 'NONE',  ( 54.99999999999999289, 515.4878487013597805, -546.7230258972048205 ) ) ;
#4100 = LINE ( 'NONE', #1350, #9635 ) ;
#4101 = CARTESIAN_POINT ( 'NONE',  ( 22.99999999999998224, 10.00000000000000000, 37.00000000000000711 ) ) ;
#4102 = ORIENTED_EDGE ( 'NONE', *, *, #5406, .T. ) ;
#4103 = DIRECTION ( 'NONE',  ( 0.000000000000000000, 0.000000000000000000, -1.000000000000000000 ) ) ;
#4104 = VECTOR ( 'NONE', #13845, 1000.000000000000000 ) ;
#4105 = DIRECTION ( 'NONE',  ( 0.000000000000000000, 0.000000000000000000, -1.000000000000000000 ) ) ;
#4106 = VERTEX_POINT ( 'NONE', #14708 ) ;
#4107 = DIRECTION ( 'NONE',  ( -0.000000000000000000, -0.000000000000000000, 1.000000000000000000 ) ) ;
#4108 = DIRECTION ( 'NONE',  ( -1.803905316987902281E-16, 1.000000000000000000, 0.000000000000000000 ) ) ;
#4109 = LINE ( 'NONE', #83, #6905 ) ;
#4110 = CARTESIAN_POINT ( 'NONE',  ( -23.00000000000000000, 68.00000000000000000, -31.00000000000005684 ) ) ;
#4111 = ORIENTED_EDGE ( 'NONE', *, *, #2574, .T. ) ;
#4112 = DIRECTION ( 'NONE',  ( 0.000000000000000000, 0.000000000000000000, 1.000000000000000000 ) ) ;
#4113 = ITEM_DEFINED_TRANSFORMATION ( 'NONE', 'NONE', #2572,  #1488 ) ;
#4114 = CIRCLE ( 'NONE', #5758, 22.49999999999999645 ) ;
#4115 = CARTESIAN_POINT ( 'NONE',  ( 19.99999999999995381, 0.000000000000000000, -36.99999999999999289 ) ) ;
#4116 = FACE_OUTER_BOUND ( 'NONE', #5359, .T. ) ;
#4117 = ORIENTED_EDGE ( 'NONE', *, *, #6866, .F. ) ;
#4118 = FACE_OUTER_BOUND ( 'NONE', #390, .T. ) ;
#4119 = UNCERTAINTY_MEASURE_WITH_UNIT (LENGTH_MEASURE( 1.000000000000000082E-05 ), #5895, 'distance_accuracy_value', 'NONE');
#4120 = DIRECTION ( 'NONE',  ( 7.213771534993946619E-17, 0.09950371902098976984, 0.9950371902099900412 ) ) ;
#4121 = EDGE_CURVE ( 'NONE', #3377, #9012, #2939, .T. ) ;
#4122 = CARTESIAN_POINT ( 'NONE',  ( 31.81980515339464333, 0.000000000000000000, 31.81980515339463622 ) ) ;
#4123 = ORIENTED_EDGE ( 'NONE', *, *, #3236, .F. ) ;
#4124 = FACE_BOUND ( 'NONE', #3631, .T. ) ;
#4125 = FACE_OUTER_BOUND ( 'NONE', #6213, .T. ) ;
#4126 = DIRECTION ( 'NONE',  ( -0.000000000000000000, -1.000000000000000000, -0.000000000000000000 ) ) ;
#4127 = VERTEX_POINT ( 'NONE', #8173 ) ;
#4128 = CIRCLE ( 'NONE', #7674, 9.000000000000007105 ) ;
#4129 = VECTOR ( 'NONE', #13781, 1000.000000000000000 ) ;
#4130 = VERTEX_POINT ( 'NONE', #14795 ) ;
#4131 = APPLICATION_CONTEXT ( 'automotive_design' ) ;
#4132 = EDGE_CURVE ( 'NONE', #11643, #13527, #6150, .T. ) ;
#4133 = VERTEX_POINT ( 'NONE', #8084 ) ;
#4134 = EDGE_CURVE ( 'NONE', #3951, #3142, #1565, .T. ) ;
#4135 = DIRECTION ( 'NONE',  ( 0.000000000000000000, 0.3420201433256757073, -0.9396926207859057634 ) ) ;
#4136 = EDGE_LOOP ( 'NONE', ( #2263, #4794, #12215, #5192 ) ) ;
#4137 = APPLICATION_PROTOCOL_DEFINITION ( 'draft international standard', 'automotive_design', 1998, #11158 ) ;
#4138 = VERTEX_POINT ( 'NONE', #6865 ) ;
#4139 = EDGE_LOOP ( 'NONE', ( #11723, #7955, #8485, #4146 ) ) ;
#4140 = FACE_OUTER_BOUND ( 'NONE', #14363, .T. ) ;
#4141 = LINE ( 'NONE', #9301, #14667 ) ;
#4142 = EDGE_CURVE ( 'NONE', #1389, #6048, #5333, .T. ) ;
#4143 = ORIENTED_EDGE ( 'NONE', *, *, #6557, .T. ) ;
#4144 = CARTESIAN_POINT ( 'NONE',  ( -36.99999999999997868, -20.00000000000000000, -19.99999999999999289 ) ) ;
#4145 = LINE ( 'NONE', #13171, #9246 ) ;
#4146 = ORIENTED_EDGE ( 'NONE', *, *, #13916, .F. ) ;
#4147 = DIRECTION ( 'NONE',  ( -1.000000000000000000, -0.000000000000000000, 0.000000000000000000 ) ) ;
#4148 = ADVANCED_FACE ( 'NONE', ( #8255 ), #15890, .T. ) ;
#4149 = EDGE_LOOP ( 'NONE', ( #10693, #16459, #9298, #9445 ) ) ;
#4150 = CARTESIAN_POINT ( 'NONE',  ( 10.00000000000000000, 372.8685141053778693, -83.18019484660869978 ) ) ;
#4151 = PLANE ( 'NONE',  #1178 ) ;
#4152 = ORIENTED_EDGE ( 'NONE', *, *, #15469, .T. ) ;
#4153 = EDGE_CURVE ( 'NONE', #12229, #10460, #14613, .T. ) ;
#4154 = AXIS2_PLACEMENT_3D ( 'NONE', #2251, #4913, #16356 ) ;
#4155 = EDGE_CURVE ( 'NONE', #7960, #10824, #14528, .T. ) ;
#4156 = EDGE_CURVE ( 'NONE', #5761, #6577, #3163, .T. ) ;
#4157 = CARTESIAN_POINT ( 'NONE',  ( 0.000000000000000000, 277.8092731128509740, -37.21049682360897748 ) ) ;
#4158 = ORIENTED_EDGE ( 'NONE', *, *, #6429, .F. ) ;
#4159 = CARTESIAN_POINT ( 'NONE',  ( 25.99999999999999645, 68.00000000000000000, -39.99999999999999289 ) ) ;
#4160 = MECHANICAL_DESIGN_GEOMETRIC_PRESENTATION_REPRESENTATION (  '', ( #10470 ), #12668 ) ;
#4161 = ORIENTED_EDGE ( 'NONE', *, *, #6459, .T. ) ;
#4162 = VERTEX_POINT ( 'NONE', #10579 ) ;
#4163 = FACE_BOUND ( 'NONE', #7037, .T. ) ;
#4164 = CARTESIAN_POINT ( 'NONE',  ( 55.99999999999989342, 493.2350855268086320, -508.1801094700848580 ) ) ;
#4165 = CARTESIAN_POINT ( 'NONE',  ( 39.72345254347677468, 303.2115381654813859, -10.00000000000000000 ) ) ;
#4166 = VECTOR ( 'NONE', #6792, 1000.000000000000000 ) ;
#4167 = EDGE_LOOP ( 'NONE', ( #3416, #13825, #12066, #7218 ) ) ;
#4168 = DIRECTION ( 'NONE',  ( -1.000000000000000000, -0.000000000000000000, -0.000000000000000000 ) ) ;
#4169 = DIRECTION ( 'NONE',  ( 0.000000000000000000, 0.000000000000000000, -1.000000000000000000 ) ) ;
#4170 = CIRCLE ( 'NONE', #9939, 22.75209553982837463 ) ;
#4171 = DIRECTION ( 'NONE',  ( 0.000000000000000000, 1.000000000000000000, 1.224646799147353207E-16 ) ) ;
#4172 = LINE ( 'NONE', #7075, #11210 ) ;
#4173 = AXIS2_PLACEMENT_3D ( 'NONE', #5529, #11804, #4259 ) ;
#4174 = ADVANCED_FACE ( 'NONE', ( #7041 ), #4226, .T. ) ;
#4175 = CARTESIAN_POINT ( 'NONE',  ( -25.99999999999999645, 68.00000000000000000, -39.99999999999999289 ) ) ;
#4176 = DIRECTION ( 'NONE',  ( 0.000000000000000000, 0.000000000000000000, -1.000000000000000000 ) ) ;
#4177 = ADVANCED_FACE ( 'NONE', ( #5496 ), #9642, .F. ) ;
#4178 = ADVANCED_FACE ( 'NONE', ( #13246 ), #12124, .T. ) ;
#4179 = DIRECTION ( 'NONE',  ( 0.000000000000000000, 0.000000000000000000, 1.000000000000000000 ) ) ;
#4180 = CARTESIAN_POINT ( 'NONE',  ( -5.000000000000000888, 2.751018388195357790E-15, -22.46376988133006236 ) ) ;
#4182 = EDGE_LOOP ( 'NONE', ( #11514, #9231, #12172, #16795 ) ) ;
#4181 = ORIENTED_EDGE ( 'NONE', *, *, #2457, .F. ) ;
#4183 = CIRCLE ( 'NONE', #6914, 9.000000000000007105 ) ;
#4184 = LINE ( 'NONE', #1607, #13043 ) ;
#4185 = CARTESIAN_POINT ( 'NONE',  ( 0.2839248860668147079, 286.0460148634705888, 37.35595106346542593 ) ) ;
#4186 = CIRCLE ( 'NONE', #1449, 2.500000000000002220 ) ;
#4187 = VECTOR ( 'NONE', #14049, 1000.000000000000000 ) ;
#4188 = FACE_OUTER_BOUND ( 'NONE', #2912, .T. ) ;
#4189 = CARTESIAN_POINT ( 'NONE',  ( 31.00000000000001776, 10.00000000000000000, -25.99999999999999645 ) ) ;
#4190 = VERTEX_POINT ( 'NONE', #10743 ) ;
#4191 = CARTESIAN_POINT ( 'NONE',  ( -55.99999999999989342, 493.2350855268086320, -508.1801094700848580 ) ) ;
#4192 = EDGE_CURVE ( 'NONE', #10633, #971, #10659, .T. ) ;
#4193 = VECTOR ( 'NONE', #6755, 1000.000000000000000 ) ;
#4194 = LINE ( 'NONE', #14682, #9802 ) ;
#4195 = ORIENTED_EDGE ( 'NONE', *, *, #3429, .T. ) ;
#4196 = DIRECTION ( 'NONE',  ( 1.000000000000000000, 0.000000000000000000, -0.000000000000000000 ) ) ;
#4197 = CARTESIAN_POINT ( 'NONE',  ( 21.99999999999998224, 8.000000000000000000, -32.99999999999999289 ) ) ;
#4198 = DIRECTION ( 'NONE',  ( -0.000000000000000000, -1.000000000000000000, -0.000000000000000000 ) ) ;
#4199 = AXIS2_PLACEMENT_3D ( 'NONE', #14036, #11709, #16768 ) ;
#4200 = CARTESIAN_POINT ( 'NONE',  ( 10.00000000000000000, 376.0487089519837127, -155.0000000000033253 ) ) ;
#4201 = STYLED_ITEM ( 'NONE', ( #14694 ), #14480 ) ;
#4202 = DIRECTION ( 'NONE',  ( 0.000000000000000000, 0.000000000000000000, 1.000000000000000000 ) ) ;
#4203 = CARTESIAN_POINT ( 'NONE',  ( -46.99999999999988631, 493.2350855268086320, -508.1801094700848580 ) ) ;
#4204 = EDGE_LOOP ( 'NONE', ( #10506, #5503, #4195, #7508 ) ) ;
#4205 = CARTESIAN_POINT ( 'NONE',  ( -45.00000000000000000, 515.4878487013597805, -571.7230258972048205 ) ) ;
#4206 = PRODUCT_DEFINITION_CONTEXT ( 'detailed design', #15862, 'design' ) ;
#4207 = VECTOR ( 'NONE', #16518, 1000.000000000000000 ) ;
#4208 = CARTESIAN_POINT ( 'NONE',  ( 5.950000000000000178, 12.65000000000000036, 0.000000000000000000 ) ) ;
#4209 = DIRECTION ( 'NONE',  ( 0.000000000000000000, 0.000000000000000000, 1.000000000000000000 ) ) ;
#4210 = VERTEX_POINT ( 'NONE', #16407 ) ;
#4211 = AXIS2_PLACEMENT_3D ( 'NONE', #14659, #2968, #14824 ) ;
#4212 = AXIS2_PLACEMENT_3D ( 'NONE', #10360, #15590, #1160 ) ;
#4213 = CYLINDRICAL_SURFACE ( 'NONE', #883, 4.999999999999997335 ) ;
#4214 = CARTESIAN_POINT ( 'NONE',  ( -40.00000000000000000, 19.00000000000000000, -26.00000000000000355 ) ) ;
#4215 = CYLINDRICAL_SURFACE ( 'NONE', #8669, 59.99999999999982947 ) ;
#4216 = VERTEX_POINT ( 'NONE', #533 ) ;
#4217 = CYLINDRICAL_SURFACE ( 'NONE', #16021, 13.69540538389601991 ) ;
#4218 = CARTESIAN_POINT ( 'NONE',  ( 75.00000000000000000, 277.8092731128509740, -37.21049682360897748 ) ) ;
#4219 = CARTESIAN_POINT ( 'NONE',  ( 40.00000000000003553, 0.000000000000000000, -25.99999999999999645 ) ) ;
#4220 = ORIENTED_EDGE ( 'NONE', *, *, #13723, .F. ) ;
#4221 = CIRCLE ( 'NONE', #8610, 3.300000000000011369 ) ;
#4222 = SURFACE_SIDE_STYLE ('',( #13241 ) ) ;
#4223 = VERTEX_POINT ( 'NONE', #12377 ) ;
#4224 = VERTEX_POINT ( 'NONE', #16327 ) ;
#4225 = CIRCLE ( 'NONE', #2846, 3.299999999999997158 ) ;
#4226 = CYLINDRICAL_SURFACE ( 'NONE', #679, 4.999999999999997335 ) ;
#4227 = AXIS2_PLACEMENT_3D ( 'NONE', #2607, #15403, #12829 ) ;
#4228 = AXIS2_PLACEMENT_3D ( 'NONE', #14281, #11529, #14203 ) ;
#4229 = ORIENTED_EDGE ( 'NONE', *, *, #16927, .T. ) ;
#4230 =( LENGTH_UNIT ( ) NAMED_UNIT ( * ) SI_UNIT ( .MILLI., .METRE. ) );
#4231 = ADVANCED_FACE ( 'NONE', ( #11173 ), #7374, .T. ) ;
#4232 = VERTEX_POINT ( 'NONE', #12465 ) ;
#4233 = AXIS2_PLACEMENT_3D ( 'NONE', #12792, #14167, #1358 ) ;
#4234 = VERTEX_POINT ( 'NONE', #11336 ) ;
#4235 = PLANE ( 'NONE',  #5237 ) ;
#4236 = CARTESIAN_POINT ( 'NONE',  ( -1.141714397801684633E-14, 214.4632308570089947, 287.5298983642209123 ) ) ;
#4237 = EDGE_CURVE ( 'NONE', #4738, #7408, #9733, .T. ) ;
#4238 = PRODUCT_DEFINITION_FORMATION_WITH_SPECIFIED_SOURCE ( 'ANY', '', #10283, .NOT_KNOWN. ) ;
#4239 = VERTEX_POINT ( 'NONE', #4811 ) ;
#4240 = CARTESIAN_POINT ( 'NONE',  ( 0.000000000000000000, 240.7889724647196488, -16.41886574335980242 ) ) ;
#4241 = AXIS2_PLACEMENT_3D ( 'NONE', #4489, #9742, #2485 ) ;
#4242 = CARTESIAN_POINT ( 'NONE',  ( 394.0000000000001137, 451.4647406485092915, -149.8062676851188257 ) ) ;
#4243 = ORIENTED_EDGE ( 'NONE', *, *, #16683, .T. ) ;
#4244 = AXIS2_PLACEMENT_3D ( 'NONE', #3108, #16157, #5680 ) ;
#4245 = CYLINDRICAL_SURFACE ( 'NONE', #378, 4.000000000000007105 ) ;
#4246 = VERTEX_POINT ( 'NONE', #13673 ) ;
#4247 = LINE ( 'NONE', #14635, #4854 ) ;
#4248 = CARTESIAN_POINT ( 'NONE',  ( 22.99999999999997513, 10.00000000000000000, 31.00000000000005684 ) ) ;
#4249 = VERTEX_POINT ( 'NONE', #12626 ) ;
#4250 = DIRECTION ( 'NONE',  ( 0.000000000000000000, 0.000000000000000000, -1.000000000000000000 ) ) ;
#4251 = ORIENTED_EDGE ( 'NONE', *, *, #9611, .T. ) ;
#4252 = DIRECTION ( 'NONE',  ( -7.888609052210118054E-31, 0.000000000000000000, 1.000000000000000000 ) ) ;
#4253 = DIRECTION ( 'NONE',  ( 0.000000000000000000, 0.000000000000000000, -1.000000000000000000 ) ) ;
#4254 = PRODUCT_DEFINITION_FORMATION_WITH_SPECIFIED_SOURCE ( 'ANY', '', #16847, .NOT_KNOWN. ) ;
#4255 = EDGE_CURVE ( 'NONE', #4694, #15712, #12738, .T. ) ;
#4256 = EDGE_CURVE ( 'NONE', #3047, #2613, #5759, .T. ) ;
#4257 = ORIENTED_EDGE ( 'NONE', *, *, #8247, .T. ) ;
#4258 = ORIENTED_EDGE ( 'NONE', *, *, #10449, .T. ) ;
#4259 = DIRECTION ( 'NONE',  ( 1.000000000000000000, 0.000000000000000000, -0.000000000000000000 ) ) ;
#4260 = VECTOR ( 'NONE', #11314, 1000.000000000000000 ) ;
#4261 = CARTESIAN_POINT ( 'NONE',  ( -55.99999999999989342, 493.2350855268086320, -508.1801094700848580 ) ) ;
#4262 = EDGE_CURVE ( 'NONE', #3296, #4760, #7119, .T. ) ;
#4263 = CARTESIAN_POINT ( 'NONE',  ( -19.00000000000001776, 10.00000000000000000, 40.00000000000000711 ) ) ;
#4264 = EDGE_CURVE ( 'NONE', #15448, #4076, #3530, .T. ) ;
#4265 = EDGE_CURVE ( 'NONE', #12820, #7289, #14003, .T. ) ;
#4267 = EDGE_CURVE ( 'NONE', #16501, #3203, #788, .T. ) ;
#4266 = DIRECTION ( 'NONE',  ( -0.000000000000000000, -0.000000000000000000, -1.000000000000000000 ) ) ;
#4268 = PRODUCT_DEFINITION_SHAPE ( 'NONE', 'NONE',  #16967 ) ;
#4269 = DIRECTION ( 'NONE',  ( 0.000000000000000000, -1.000000000000000000, 0.000000000000000000 ) ) ;
#4270 = DIRECTION ( 'NONE',  ( -1.000000000000000000, 0.000000000000000000, -0.000000000000000000 ) ) ;
#4271 = DIRECTION ( 'NONE',  ( -0.000000000000000000, -1.000000000000000000, 0.000000000000000000 ) ) ;
#4272 = DIRECTION ( 'NONE',  ( 0.000000000000000000, 0.000000000000000000, -1.000000000000000000 ) ) ;
#4273 = CARTESIAN_POINT ( 'NONE',  ( -22.99999999999999645, 68.00000000000000000, -36.99999999999999289 ) ) ;
#4274 = AXIS2_PLACEMENT_3D ( 'NONE', #12692, #5194, #3507 ) ;
#4275 = FACE_OUTER_BOUND ( 'NONE', #15391, .T. ) ;
#4276 = CARTESIAN_POINT ( 'NONE',  ( -46.99999999999988631, 493.2350855268092573, -585.2659423243250103 ) ) ;
#4278 = VERTEX_POINT ( 'NONE', #15037 ) ;
#4277 = ORIENTED_EDGE ( 'NONE', *, *, #1000, .T. ) ;
#4279 = LINE ( 'NONE', #13383, #16058 ) ;
#4280 = EDGE_CURVE ( 'NONE', #10225, #7947, #866, .T. ) ;
#4281 = CYLINDRICAL_SURFACE ( 'NONE', #11553, 84.99999999999997158 ) ;
#4282 = CARTESIAN_POINT ( 'NONE',  ( -31.00000000000003553, 11.00000000000000000, -26.00000000000000355 ) ) ;
#4283 = EDGE_CURVE ( 'NONE', #2908, #2740, #2143, .T. ) ;
#4284 = DIRECTION ( 'NONE',  ( 0.000000000000000000, 0.000000000000000000, 1.000000000000000000 ) ) ;
#4285 = ADVANCED_FACE ( 'NONE', ( #8691 ), #6406, .T. ) ;
#4286 = AXIS2_PLACEMENT_3D ( 'NONE', #7464, #11348, #10073 ) ;
#4287 = ORIENTED_EDGE ( 'NONE', *, *, #14755, .F. ) ;
#4288 = VECTOR ( 'NONE', #9575, 1000.000000000000000 ) ;
#4289 = EDGE_CURVE ( 'NONE', #14833, #10297, #3276, .T. ) ;
#4290 = DIRECTION ( 'NONE',  ( -1.000000000000000000, -0.000000000000000000, -0.000000000000000000 ) ) ;
#4291 = CARTESIAN_POINT ( 'NONE',  ( 31.99999999999998579, 6.000000000000000000, 25.99999999999999645 ) ) ;
#4292 = ORIENTED_EDGE ( 'NONE', *, *, #13510, .F. ) ;
#4293 = DIRECTION ( 'NONE',  ( -1.000000000000000000, -0.000000000000000000, 0.000000000000000000 ) ) ;
#4294 = DIRECTION ( 'NONE',  ( -0.003530072958128175308, 0.9999937692730440641, 0.000000000000000000 ) ) ;
#4295 = DIRECTION ( 'NONE',  ( -0.000000000000000000, -1.000000000000000000, -0.000000000000000000 ) ) ;
#4296 = CARTESIAN_POINT ( 'NONE',  ( 20.99999999999996092, 0.000000000000000000, 35.00000000000000711 ) ) ;
#4297 = DIRECTION ( 'NONE',  ( 0.000000000000000000, 0.000000000000000000, -1.000000000000000000 ) ) ;
#4298 = DIRECTION ( 'NONE',  ( -0.000000000000000000, -1.000000000000000000, -0.000000000000000000 ) ) ;
#4299 = VERTEX_POINT ( 'NONE', #5930 ) ;
#4300 = VECTOR ( 'NONE', #8168, 1000.000000000000000 ) ;
#4301 = FACE_OUTER_BOUND ( 'NONE', #6520, .T. ) ;
#4302 = CIRCLE ( 'NONE', #13630, 0.9999999999999983347 ) ;
#4303 = LINE ( 'NONE', #3089, #9463 ) ;
#4304 = PLANE ( 'NONE',  #5550 ) ;
#4305 = ORIENTED_EDGE ( 'NONE', *, *, #14674, .T. ) ;
#4306 = FACE_OUTER_BOUND ( 'NONE', #6269, .T. ) ;
#4307 = UNCERTAINTY_MEASURE_WITH_UNIT (LENGTH_MEASURE( 1.000000000000000082E-05 ), #12057, 'distance_accuracy_value', 'NONE');
#4308 = PLANE ( 'NONE',  #15751 ) ;
#4309 = CIRCLE ( 'NONE', #14172, 13.69540538389601991 ) ;
#4310 = DIRECTION ( 'NONE',  ( -1.000000000000000000, -0.000000000000000000, -0.000000000000000000 ) ) ;
#4311 = ORIENTED_EDGE ( 'NONE', *, *, #13377, .F. ) ;
#4312 = CIRCLE ( 'NONE', #202, 9.999999999999994671 ) ;
#4313 = FACE_OUTER_BOUND ( 'NONE', #2320, .T. ) ;
#4314 = DIRECTION ( 'NONE',  ( 1.000000000000000000, 0.000000000000000000, 0.000000000000000000 ) ) ;
#4315 = PLANE ( 'NONE',  #8403 ) ;
#4316 = VERTEX_POINT ( 'NONE', #8601 ) ;
#4317 = CARTESIAN_POINT ( 'NONE',  ( -33.99999999999997158, 3.000000000000000000, -22.99999999999999645 ) ) ;
#4318 = VERTEX_POINT ( 'NONE', #3198 ) ;
#4319 = ORIENTED_EDGE ( 'NONE', *, *, #6846, .F. ) ;
#4320 = PLANE ( 'NONE',  #13579 ) ;
#4321 = ORIENTED_EDGE ( 'NONE', *, *, #7702, .F. ) ;
#4322 = ADVANCED_FACE ( 'NONE', ( #8510 ), #15218, .T. ) ;
#4323 = PRODUCT_CONTEXT ( 'NONE', #13576, 'mechanical' ) ;
#4324 = VECTOR ( 'NONE', #1148, 1000.000000000000000 ) ;
#4325 = AXIS2_PLACEMENT_3D ( 'NONE', #14015, #6015, #12478 ) ;
#4326 = ORIENTED_EDGE ( 'NONE', *, *, #7050, .F. ) ;
#4327 = ADVANCED_FACE ( 'NONE', ( #1979 ), #7205, .F. ) ;
#4328 = ORIENTED_EDGE ( 'NONE', *, *, #10365, .F. ) ;
#4329 = CARTESIAN_POINT ( 'NONE',  ( 35.00000000000000711, 0.000000000000000000, -35.00000000000000711 ) ) ;
#4330 = DIRECTION ( 'NONE',  ( 0.000000000000000000, 0.000000000000000000, 1.000000000000000000 ) ) ;
#4331 = EDGE_LOOP ( 'NONE', ( #2314, #8097, #16618, #6428 ) ) ;
#4332 = CARTESIAN_POINT ( 'NONE',  ( 10.00000000000000000, 372.8685141053783241, -150.1198051533980049 ) ) ;
#4333 = DIRECTION ( 'NONE',  ( 1.000000000000000000, 0.000000000000000000, 0.000000000000000000 ) ) ;
#4334 = VERTEX_POINT ( 'NONE', #13924 ) ;
#4335 = AXIS2_PLACEMENT_3D ( 'NONE', #3949, #10718, #10905 ) ;
#4336 = ORIENTED_EDGE ( 'NONE', *, *, #12710, .T. ) ;
#4337 = CARTESIAN_POINT ( 'NONE',  ( 46.99999999999988631, 549.5810598491749488, -561.6352214130889706 ) ) ;
#4338 = CARTESIAN_POINT ( 'NONE',  ( 7.000000000000001776, 380.0000000000000000, -75.00000000000000000 ) ) ;
#4339 = EDGE_LOOP ( 'NONE', ( #5513, #8062, #7972, #3794 ) ) ;
#4340 = ORIENTED_EDGE ( 'NONE', *, *, #10274, .T. ) ;
#4341 =( NAMED_UNIT ( * ) PLANE_ANGLE_UNIT ( ) SI_UNIT ( $, .RADIAN. ) );
#4342 = EDGE_CURVE ( 'NONE', #14244, #16161, #2043, .T. ) ;
#4343 = LINE ( 'NONE', #6890, #4288 ) ;
#4344 = ORIENTED_EDGE ( 'NONE', *, *, #14710, .F. ) ;
#4345 = VERTEX_POINT ( 'NONE', #952 ) ;
#4346 = DIRECTION ( 'NONE',  ( 1.000000000000000000, -0.000000000000000000, 0.000000000000000000 ) ) ;
#4347 = AXIS2_PLACEMENT_3D ( 'NONE', #10256, #14032, #8538 ) ;
#4348 = FACE_OUTER_BOUND ( 'NONE', #5610, .T. ) ;
#4349 = CARTESIAN_POINT ( 'NONE',  ( -23.00000000000002842, 10.00000000000000000, -36.99999999999999289 ) ) ;
#4350 = CARTESIAN_POINT ( 'NONE',  ( 55.99999999999989342, 473.6663340069157471, -531.5012393965008641 ) ) ;
#4351 = LINE ( 'NONE', #3054, #2832 ) ;
#4352 = ADVANCED_FACE ( 'NONE', ( #15548 ), #1115, .T. ) ;
#4353 = LINE ( 'NONE', #10784, #13701 ) ;
#4354 = LINE ( 'NONE', #8204, #2158 ) ;
#4355 = DIRECTION ( 'NONE',  ( 0.000000000000000000, 0.000000000000000000, -1.000000000000000000 ) ) ;
#4356 = LINE ( 'NONE', #12078, #70 ) ;
#4357 = FACE_OUTER_BOUND ( 'NONE', #722, .T. ) ;
#4358 = VECTOR ( 'NONE', #445, 1000.000000000000227 ) ;
#4359 = CARTESIAN_POINT ( 'NONE',  ( -23.00000000000002487, 6.000000000000000000, -36.99999999999999289 ) ) ;
#4361 = ORIENTED_EDGE ( 'NONE', *, *, #7804, .F. ) ;
#4360 = ORIENTED_EDGE ( 'NONE', *, *, #7797, .F. ) ;
#4362 = ADVANCED_FACE ( 'NONE', ( #1037 ), #6975, .T. ) ;
#4363 = LINE ( 'NONE', #9928, #10849 ) ;
#4364 = CARTESIAN_POINT ( 'NONE',  ( 0.7365999999999665038, 289.4632308570086252, 37.52989836422097625 ) ) ;
#4365 = DIRECTION ( 'NONE',  ( 0.000000000000000000, 0.000000000000000000, -1.000000000000000000 ) ) ;
#4366 = DIRECTION ( 'NONE',  ( 0.000000000000000000, 1.000000000000000000, 0.000000000000000000 ) ) ;
#4367 = EDGE_LOOP ( 'NONE', ( #10143, #14132, #541, #14955 ) ) ;
#4368 = VECTOR ( 'NONE', #11493, 1000.000000000000000 ) ;
#4369 = CARTESIAN_POINT ( 'NONE',  ( 10.00000000000000000, 306.0487089519832011, -80.00000000000380851 ) ) ;
#4370 = LINE ( 'NONE', #12092, #12797 ) ;
#4372 = ADVANCED_FACE ( 'NONE', ( #11503 ), #12961, .F. ) ;
#4371 = ORIENTED_EDGE ( 'NONE', *, *, #16642, .T. ) ;
#4373 = DIRECTION ( 'NONE',  ( 0.000000000000000000, 0.000000000000000000, 1.000000000000000000 ) ) ;
#4374 = DIRECTION ( 'NONE',  ( 1.000000000000000000, -0.000000000000000000, -0.000000000000000000 ) ) ;
#4375 = CARTESIAN_POINT ( 'NONE',  ( 414.7091847417151484, 350.3558646104334571, -10.00000000000000000 ) ) ;
#4376 = CARTESIAN_POINT ( 'NONE',  ( 49.99999999999999289, 515.4878487013597805, -486.7230258972047636 ) ) ;
#4377 = DIRECTION ( 'NONE',  ( 1.000000000000000000, 0.000000000000000000, 0.000000000000000000 ) ) ;
#4378 = CARTESIAN_POINT ( 'NONE',  ( 0.000000000000000000, 66.00000000000000000, 0.000000000000000000 ) ) ;
#4379 = ORIENTED_EDGE ( 'NONE', *, *, #9100, .F. ) ;
#4380 = EDGE_CURVE ( 'NONE', #16035, #742, #6172, .T. ) ;
#4381 = ADVANCED_FACE ( 'NONE', ( #15460 ), #16903, .T. ) ;
#4382 = ADVANCED_FACE ( 'NONE', ( #10469 ), #5878, .T. ) ;
#4383 = LINE ( 'NONE', #258, #16317 ) ;
#4384 = EDGE_CURVE ( 'NONE', #11352, #295, #7543, .T. ) ;
#4385 = CYLINDRICAL_SURFACE ( 'NONE', #8498, 2.999999999999995559 ) ;
#4386 = LINE ( 'NONE', #12108, #5835 ) ;
#4387 = CIRCLE ( 'NONE', #13978, 4.999999999999997335 ) ;
#4388 = ORIENTED_EDGE ( 'NONE', *, *, #6439, .F. ) ;
#4389 = DIRECTION ( 'NONE',  ( -0.000000000000000000, 1.000000000000000000, -0.000000000000000000 ) ) ;
#4390 = DIRECTION ( 'NONE',  ( 0.000000000000000000, 0.000000000000000000, 1.000000000000000000 ) ) ;
#4391 = ORIENTED_EDGE ( 'NONE', *, *, #6533, .T. ) ;
#4392 = CARTESIAN_POINT ( 'NONE',  ( -55.99999999999989342, 559.9933750504617365, -546.7230258972048205 ) ) ;
#4393 = CARTESIAN_POINT ( 'NONE',  ( 40.00000000000003553, 3.000000000000000000, 20.00000000000000355 ) ) ;
#4394 = CARTESIAN_POINT ( 'NONE',  ( 10.00000000000000000, 309.2289037985885898, -83.18019484660915452 ) ) ;
#4395 = ORIENTED_EDGE ( 'NONE', *, *, #15894, .T. ) ;
#4396 = FILL_AREA_STYLE ('',( #8079 ) ) ;
#4397 = ORIENTED_EDGE ( 'NONE', *, *, #15958, .F. ) ;
#4398 = ORIENTED_EDGE ( 'NONE', *, *, #13882, .T. ) ;
#4399 = VECTOR ( 'NONE', #6822, 1000.000000000000000 ) ;
#4400 = DIRECTION ( 'NONE',  ( 0.000000000000000000, 0.000000000000000000, -1.000000000000000000 ) ) ;
#4401 = CIRCLE ( 'NONE', #4930, 0.6999999999999992895 ) ;
#4402 = EDGE_CURVE ( 'NONE', #10404, #8973, #11368, .T. ) ;
#4403 = ORIENTED_EDGE ( 'NONE', *, *, #12129, .F. ) ;
#4404 = APPLICATION_PROTOCOL_DEFINITION ( 'draft international standard', 'automotive_design', 1998, #6417 ) ;
#4405 = ORIENTED_EDGE ( 'NONE', *, *, #4904, .F. ) ;
#4406 = ORIENTED_EDGE ( 'NONE', *, *, #1627, .F. ) ;
#4407 = DIRECTION ( 'NONE',  ( 6.123031769111888756E-17, -1.000000000000000000, -3.749151804555344967E-33 ) ) ;
#4408 = DIRECTION ( 'NONE',  ( -0.000000000000000000, -0.000000000000000000, 1.000000000000000000 ) ) ;
#4409 = VECTOR ( 'NONE', #5171, 1000.000000000000000 ) ;
#4410 = ORIENTED_EDGE ( 'NONE', *, *, #4121, .F. ) ;
#4412 = DIRECTION ( 'NONE',  ( 0.000000000000000000, 0.000000000000000000, -1.000000000000000000 ) ) ;
#4411 = AXIS2_PLACEMENT_3D ( 'NONE', #11905, #5537, #4270 ) ;
#4413 = DIRECTION ( 'NONE',  ( 0.000000000000000000, 0.000000000000000000, -1.000000000000000000 ) ) ;
#4414 = VERTEX_POINT ( 'NONE', #2479 ) ;
#4415 = FACE_OUTER_BOUND ( 'NONE', #13948, .T. ) ;
#4416 = ORIENTED_EDGE ( 'NONE', *, *, #2051, .T. ) ;
#4417 = DIRECTION ( 'NONE',  ( 0.000000000000000000, 0.000000000000000000, 1.000000000000000000 ) ) ;
#4418 = CARTESIAN_POINT ( 'NONE',  ( 10.00000000000000000, 306.0487089519837696, -155.0000000000038369 ) ) ;
#4419 = ORIENTED_EDGE ( 'NONE', *, *, #9354, .T. ) ;
#4420 = EDGE_LOOP ( 'NONE', ( #14868, #13648, #5990, #4601, #12019, #15245, #8016, #2666 ) ) ;
#4421 = LINE ( 'NONE', #9663, #8111 ) ;
#4422 = VERTEX_POINT ( 'NONE', #14087 ) ;
#4423 = ORIENTED_EDGE ( 'NONE', *, *, #7781, .T. ) ;
#4424 = CARTESIAN_POINT ( 'NONE',  ( -2.694300560877699535, 39.66622868771214883, 9.110264267939502503 ) ) ;
#4425 = DIRECTION ( 'NONE',  ( -1.000000000000000000, 0.000000000000000000, 0.000000000000000000 ) ) ;
#4426 = DIRECTION ( 'NONE',  ( -0.000000000000000000, -1.000000000000000000, -0.000000000000000000 ) ) ;
#4427 = CARTESIAN_POINT ( 'NONE',  ( -37.00000000000000711, 10.00000000000000000, -18.00000000000000355 ) ) ;
#4428 = FACE_OUTER_BOUND ( 'NONE', #12678, .T. ) ;
#4429 = AXIS2_PLACEMENT_3D ( 'NONE', #10359, #15588, #3824 ) ;
#4430 = CARTESIAN_POINT ( 'NONE',  ( 0.000000000000000000, 340.8211049126788907, -341.7267989266199493 ) ) ;
#4431 = CARTESIAN_POINT ( 'NONE',  ( 46.99999999999988631, 523.2161522479893847, -576.8570079137933817 ) ) ;
#4432 = DIRECTION ( 'NONE',  ( 0.000000000000000000, -1.000000000000000000, 0.000000000000000000 ) ) ;
#4433 = DIRECTION ( 'NONE',  ( 0.000000000000000000, 0.000000000000000000, -1.000000000000000000 ) ) ;
#4434 = CARTESIAN_POINT ( 'NONE',  ( 394.0000000000001137, 339.4485271457189128, -10.62862937063367852 ) ) ;
#4436 = ORIENTED_EDGE ( 'NONE', *, *, #4003, .T. ) ;
#4435 = ORIENTED_EDGE ( 'NONE', *, *, #14239, .F. ) ;
#4437 = CARTESIAN_POINT ( 'NONE',  ( 0.000000000000000000, 0.000000000000000000, 0.000000000000000000 ) ) ;
#4438 = LINE ( 'NONE', #15256, #14306 ) ;
#4439 = ADVANCED_FACE ( 'NONE', ( #3862 ), #9101, .F. ) ;
#4440 = EDGE_CURVE ( 'NONE', #4232, #4991, #4966, .T. ) ;
#4441 = CARTESIAN_POINT ( 'NONE',  ( 1.286622718088548112E-12, 258.8496290447203023, 286.9685381829918924 ) ) ;
#4442 = CARTESIAN_POINT ( 'NONE',  ( -55.99999999999988631, 172.2913238082672933, 146.1547335252150788 ) ) ;
#4443 = VERTEX_POINT ( 'NONE', #5217 ) ;
#4444 = VECTOR ( 'NONE', #15546, 1000.000000000000000 ) ;
#4445 = VECTOR ( 'NONE', #5211, 1000.000000000000000 ) ;
#4446 = EDGE_CURVE ( 'NONE', #15081, #2860, #9192, .T. ) ;
#4447 = CARTESIAN_POINT ( 'NONE',  ( 22.99999999999998224, 0.000000000000000000, 37.00000000000000711 ) ) ;
#4448 = EDGE_LOOP ( 'NONE', ( #4504, #14702, #8506, #7747 ) ) ;
#4449 = DIRECTION ( 'NONE',  ( -0.000000000000000000, 1.000000000000000000, -0.000000000000000000 ) ) ;
#4450 = CARTESIAN_POINT ( 'NONE',  ( 5.945602903476760126, 13.89560290347679938, 0.000000000000000000 ) ) ;
#4451 = CARTESIAN_POINT ( 'NONE',  ( 0.000000000000000000, 66.00000000000000000, -5.741599279633704455E-16 ) ) ;
#4452 = AXIS2_PLACEMENT_3D ( 'NONE', #13231, #1463, #11946 ) ;
#4453 = DIRECTION ( 'NONE',  ( 1.000000000000000000, -0.000000000000000000, 0.000000000000000000 ) ) ;
#4454 = ORIENTED_EDGE ( 'NONE', *, *, #67, .T. ) ;
#4455 = CARTESIAN_POINT ( 'NONE',  ( -54.99999999999999289, 515.4878487013597805, -359.2230258972048773 ) ) ;
#4456 = AXIS2_PLACEMENT_3D ( 'NONE', #16179, #16268, #11030 ) ;
#4457 = LINE ( 'NONE', #9449, #7106 ) ;
#4458 = EDGE_CURVE ( 'NONE', #15367, #9686, #11382, .T. ) ;
#4459 = APPLICATION_CONTEXT ( 'automotive_design' ) ;
#4460 = CARTESIAN_POINT ( 'NONE',  ( -33.99999999999997158, 0.000000000000000000, -22.99999999999999645 ) ) ;
#4461 = CIRCLE ( 'NONE', #15431, 2.500000000000002220 ) ;
#4462 = EDGE_LOOP ( 'NONE', ( #15817, #9352, #4774, #2195 ) ) ;
#4463 = CARTESIAN_POINT ( 'NONE',  ( -46.99999999999988631, 549.5810598491749488, -575.3306267969850296 ) ) ;
#4464 = EDGE_CURVE ( 'NONE', #5920, #11543, #8849, .T. ) ;
#4465 = EDGE_CURVE ( 'NONE', #5021, #882, #3173, .T. ) ;
#4466 = DIRECTION ( 'NONE',  ( 0.000000000000000000, 0.000000000000000000, 1.000000000000000000 ) ) ;
#4467 = ORIENTED_EDGE ( 'NONE', *, *, #8686, .T. ) ;
#4468 = DIRECTION ( 'NONE',  ( 0.000000000000000000, 0.9950371902099902632, -0.09950371902098713306 ) ) ;
#4469 = ADVANCED_FACE ( 'NONE', ( #8937, #14178 ), #7627, .T. ) ;
#4470 = VECTOR ( 'NONE', #13960, 1000.000000000000000 ) ;
#4471 = PRESENTATION_LAYER_ASSIGNMENT (  '', '', ( #14618 ) ) ;
#4472 = CARTESIAN_POINT ( 'NONE',  ( 22.99999999999995737, 3.000000000000000000, -33.99999999999998579 ) ) ;
#4473 = DIRECTION ( 'NONE',  ( -1.000000000000000000, 0.000000000000000000, 7.709882115452498874E-16 ) ) ;
#4474 = ORIENTED_EDGE ( 'NONE', *, *, #11704, .T. ) ;
#4475 = CARTESIAN_POINT ( 'NONE',  ( 37.00000000000003553, 0.000000000000000000, 23.00000000000000355 ) ) ;
#4476 = EDGE_LOOP ( 'NONE', ( #10747, #8446, #9392, #13016 ) ) ;
#4477 = VERTEX_POINT ( 'NONE', #12021 ) ;
#4478 = VECTOR ( 'NONE', #465, 1000.000000000000000 ) ;
#4479 = CARTESIAN_POINT ( 'NONE',  ( -37.00000000000000000, 0.000000000000000000, 23.00000000000000355 ) ) ;
#4480 = ORIENTED_EDGE ( 'NONE', *, *, #8243, .F. ) ;
#4481 = SHAPE_DEFINITION_REPRESENTATION ( #11358, #6937 ) ;
#4482 = CIRCLE ( 'NONE', #3701, 18.49999999999998934 ) ;
#4483 = VECTOR ( 'NONE', #12235, 1000.000000000000000 ) ;
#4484 = ORIENTED_EDGE ( 'NONE', *, *, #13398, .T. ) ;
#4485 = CARTESIAN_POINT ( 'NONE',  ( 30.99999999999996092, 3.000000000000000000, -30.99999999999999289 ) ) ;
#4486 = VERTEX_POINT ( 'NONE', #15959 ) ;
#4487 = CARTESIAN_POINT ( 'NONE',  ( -22.00000000000001776, 10.00000000000000000, 32.00000000000000711 ) ) ;
#4488 = EDGE_CURVE ( 'NONE', #14135, #7845, #4383, .T. ) ;
#4489 = CARTESIAN_POINT ( 'NONE',  ( 46.99999999999988631, 493.2350855268092573, -585.2659423243250103 ) ) ;
#4490 = AXIS2_PLACEMENT_3D ( 'NONE', #1813, #7034, #3099 ) ;
#4491 = EDGE_CURVE ( 'NONE', #16266, #1294, #14122, .T. ) ;
#4492 = ORIENTED_EDGE ( 'NONE', *, *, #15269, .T. ) ;
#4493 = CARTESIAN_POINT ( 'NONE',  ( -23.00000000000003197, 0.000000000000000000, 34.00000000000000711 ) ) ;
#4494 = ADVANCED_FACE ( 'NONE', ( #14776 ), #1547, .F. ) ;
#4495 = LINE ( 'NONE', #466, #16908 ) ;
#4496 = ORIENTED_EDGE ( 'NONE', *, *, #15919, .F. ) ;
#4497 = VECTOR ( 'NONE', #15229, 1000.000000000000000 ) ;
#4498 = VECTOR ( 'NONE', #2095, 1000.000000000000000 ) ;
#4499 = CONICAL_SURFACE ( 'NONE', #6675, 14.92500000000000071, 1.076854957875310381 ) ;
#4500 = ORIENTED_EDGE ( 'NONE', *, *, #4121, .T. ) ;
#4501 = CARTESIAN_POINT ( 'NONE',  ( -39.99999999999999289, 0.000000000000000000, 34.99999999999997868 ) ) ;
#4502 = ORIENTED_EDGE ( 'NONE', *, *, #5179, .F. ) ;
#4503 = AXIS2_PLACEMENT_3D ( 'NONE', #10406, #1384, #5076 ) ;
#4504 = ORIENTED_EDGE ( 'NONE', *, *, #8793, .T. ) ;
#4505 = AXIS2_PLACEMENT_3D ( 'NONE', #4707, #7443, #13743 ) ;
#4506 = VERTEX_POINT ( 'NONE', #11939 ) ;
#4507 = AXIS2_PLACEMENT_3D ( 'NONE', #4475, #4558, #5927 ) ;
#4508 = VERTEX_POINT ( 'NONE', #4205 ) ;
#4510 = CARTESIAN_POINT ( 'NONE',  ( 0.000000000000000000, 26.00000000000000000, 0.000000000000000000 ) ) ;
#4509 = AXIS2_PLACEMENT_3D ( 'NONE', #1368, #5088, #13530 ) ;
#4511 = CIRCLE ( 'NONE', #14106, 17.52499999999999858 ) ;
#4512 = DIRECTION ( 'NONE',  ( 0.000000000000000000, 0.000000000000000000, 1.000000000000000000 ) ) ;
#4513 = FACE_OUTER_BOUND ( 'NONE', #6047, .T. ) ;
#4514 = LINE ( 'NONE', #398, #11463 ) ;
#4515 = AXIS2_PLACEMENT_3D ( 'NONE', #12716, #13058, #16818 ) ;
#4516 = PLANE ( 'NONE',  #3675 ) ;
#4517 = CARTESIAN_POINT ( 'NONE',  ( 10.00000000000000000, 306.0487089519832011, -75.00000000000380851 ) ) ;
#4518 = FACE_BOUND ( 'NONE', #6844, .T. ) ;
#4519 = EDGE_LOOP ( 'NONE', ( #11471, #5686, #6192, #8707 ) ) ;
#4520 = DIRECTION ( 'NONE',  ( 1.000000000000000000, -0.000000000000000000, 0.000000000000000000 ) ) ;
#4521 = CARTESIAN_POINT ( 'NONE',  ( 10.00000000000000000, 1.106257942394396377E-12, -155.0000000000060254 ) ) ;
#4522 = CARTESIAN_POINT ( 'NONE',  ( 55.99999999999989342, 523.2161522479888163, -502.8936384967199729 ) ) ;
#4523 = VECTOR ( 'NONE', #10649, 1000.000000000000000 ) ;
#4524 = DIRECTION ( 'NONE',  ( 0.000000000000000000, -1.321694076934710402E-16, 1.000000000000000000 ) ) ;
#4526 = EDGE_LOOP ( 'NONE', ( #15153, #9628, #11313, #8607 ) ) ;
#4525 = ORIENTED_EDGE ( 'NONE', *, *, #3946, .T. ) ;
#4527 = DIRECTION ( 'NONE',  ( 3.491481338843133355E-15, -0.9950371902099891530, -0.09950371902099770793 ) ) ;
#4528 = CIRCLE ( 'NONE', #14685, 25.25038683781155413 ) ;
#4530 = ADVANCED_FACE ( 'NONE', ( #2735 ), #1366, .T. ) ;
#4529 = AXIS2_PLACEMENT_3D ( 'NONE', #7100, #7268, #3255 ) ;
#4531 = CARTESIAN_POINT ( 'NONE',  ( 1.223489862255693833E-15, 0.000000000000000000, -75.00000000000000000 ) ) ;
#4532 = DIRECTION ( 'NONE',  ( 0.000000000000000000, 0.000000000000000000, 1.000000000000000000 ) ) ;
#4533 = CARTESIAN_POINT ( 'NONE',  ( -31.00000000000003553, 19.00000000000000000, 25.99999999999999645 ) ) ;
#4534 = ORIENTED_EDGE ( 'NONE', *, *, #5200, .F. ) ;
#4535 = EDGE_CURVE ( 'NONE', #3545, #4994, #6936, .T. ) ;
#4536 = DIRECTION ( 'NONE',  ( 0.000000000000000000, 1.000000000000000000, 0.000000000000000000 ) ) ;
#4537 = ORIENTED_EDGE ( 'NONE', *, *, #3605, .T. ) ;
#4538 = DIRECTION ( 'NONE',  ( 0.000000000000000000, 1.000000000000000000, 0.000000000000000000 ) ) ;
#4539 = VECTOR ( 'NONE', #1525, 1000.000000000000000 ) ;
#4540 = LINE ( 'NONE', #13808, #16092 ) ;
#4541 = CARTESIAN_POINT ( 'NONE',  ( 25.99999999999998224, 0.000000000000000000, -31.00000000000003197 ) ) ;
#4542 = CARTESIAN_POINT ( 'NONE',  ( -39.99999999999999289, 8.000000000000000000, 34.99999999999997868 ) ) ;
#4543 = CARTESIAN_POINT ( 'NONE',  ( 21.00000000000000000, 19.00000000000000000, -31.00000000000003908 ) ) ;
#4544 = ORIENTED_EDGE ( 'NONE', *, *, #2153, .T. ) ;
#4545 = DIRECTION ( 'NONE',  ( -1.000000000000000000, -0.000000000000000000, -0.000000000000000000 ) ) ;
#4546 = EDGE_CURVE ( 'NONE', #12299, #583, #433, .T. ) ;
#4547 = DIRECTION ( 'NONE',  ( 0.000000000000000000, 0.000000000000000000, 1.000000000000000000 ) ) ;
#4548 = AXIS2_PLACEMENT_3D ( 'NONE', #4122, #13330, #14697 ) ;
#4549 = EDGE_LOOP ( 'NONE', ( #10948, #9125, #11985, #6566 ) ) ;
#4550 = CARTESIAN_POINT ( 'NONE',  ( -40.00000000000000711, 0.000000000000000000, -26.00000000000000000 ) ) ;
#4551 = FACE_BOUND ( 'NONE', #8407, .T. ) ;
#4552 = ORIENTED_EDGE ( 'NONE', *, *, #7797, .T. ) ;
#4553 = DIRECTION ( 'NONE',  ( -0.000000000000000000, -1.000000000000000000, -0.000000000000000000 ) ) ;
#4554 = FACE_OUTER_BOUND ( 'NONE', #3524, .T. ) ;
#4555 = ORIENTED_EDGE ( 'NONE', *, *, #12489, .F. ) ;
#4556 = EDGE_CURVE ( 'NONE', #13387, #10318, #13595, .T. ) ;
#4557 = AXIS2_PLACEMENT_3D ( 'NONE', #15693, #9182, #14416 ) ;
#4558 = DIRECTION ( 'NONE',  ( -0.000000000000000000, -1.000000000000000000, 0.000000000000000000 ) ) ;
#4559 = ORIENTED_EDGE ( 'NONE', *, *, #9845, .F. ) ;
#4560 = ORIENTED_EDGE ( 'NONE', *, *, #6073, .T. ) ;
#4561 = CARTESIAN_POINT ( 'NONE',  ( -55.99999999999989342, 493.2350855268086320, -508.1801094700848580 ) ) ;
#4562 = CONTEXT_DEPENDENT_SHAPE_REPRESENTATION ( #6313, #9473 ) ;
#4563 = EDGE_CURVE ( 'NONE', #3015, #1977, #5312, .T. ) ;
#4564 = FACE_OUTER_BOUND ( 'NONE', #1305, .T. ) ;
#4565 = AXIS2_PLACEMENT_3D ( 'NONE', #11648, #11554, #15347 ) ;
#4566 = ORIENTED_EDGE ( 'NONE', *, *, #4767, .T. ) ;
#4567 = AXIS2_PLACEMENT_3D ( 'NONE', #14165, #15447, #6318 ) ;
#4568 = CARTESIAN_POINT ( 'NONE',  ( -20.00000000000003197, 3.000000000000000000, 40.00000000000000711 ) ) ;
#4569 = CARTESIAN_POINT ( 'NONE',  ( 0.7365999999999783832, 260.4765148507123058, 287.1312267635911439 ) ) ;
#4570 = ORIENTED_EDGE ( 'NONE', *, *, #4605, .T. ) ;
#4571 = DIRECTION ( 'NONE',  ( 1.000000000000000000, 0.000000000000000000, 0.000000000000000000 ) ) ;
#4572 = DIRECTION ( 'NONE',  ( -1.000000000000000000, 0.000000000000000000, 0.000000000000000000 ) ) ;
#4573 = ORIENTED_EDGE ( 'NONE', *, *, #16215, .T. ) ;
#4574 = ADVANCED_FACE ( 'NONE', ( #4301 ), #10908, .T. ) ;
#4575 = FACE_OUTER_BOUND ( 'NONE', #15345, .T. ) ;
#4576 = EDGE_LOOP ( 'NONE', ( #6800, #9668, #5639, #5596 ) ) ;
#4577 = ORIENTED_EDGE ( 'NONE', *, *, #167, .T. ) ;
#4578 = VECTOR ( 'NONE', #5007, 1000.000000000000000 ) ;
#4579 = CIRCLE ( 'NONE', #10068, 3.299999999999997158 ) ;
#4580 = EDGE_LOOP ( 'NONE', ( #16686, #7912, #14927, #5671 ) ) ;
#4581 = EDGE_CURVE ( 'NONE', #15921, #2814, #4797, .T. ) ;
#4582 = EDGE_CURVE ( 'NONE', #7474, #7690, #2050, .T. ) ;
#4583 = EDGE_CURVE ( 'NONE', #394, #16829, #5345, .T. ) ;
#4584 = EDGE_CURVE ( 'NONE', #9725, #7810, #6159, .T. ) ;
#4585 = ORIENTED_EDGE ( 'NONE', *, *, #13411, .F. ) ;
#4586 =( REPRESENTATION_RELATIONSHIP ('NONE','NONE', #15277, #12962 ) REPRESENTATION_RELATIONSHIP_WITH_TRANSFORMATION ( #9194 )SHAPE_REPRESENTATION_RELATIONSHIP( ) );
#4587 = VERTEX_POINT ( 'NONE', #10561 ) ;
#4588 = LINE ( 'NONE', #1847, #3901 ) ;
#4589 = DIRECTION ( 'NONE',  ( -1.000000000000000000, -0.000000000000000000, -0.000000000000000000 ) ) ;
#4590 = LINE ( 'NONE', #10002, #381 ) ;
#4591 = VECTOR ( 'NONE', #6083, 1000.000000000000000 ) ;
#4592 = CARTESIAN_POINT ( 'NONE',  ( 40.00000000000000711, 11.00000000000000000, 34.99999999999997868 ) ) ;
#4593 = CARTESIAN_POINT ( 'NONE',  ( 32.99999999999998579, 8.000000000000000000, 25.99999999999999645 ) ) ;
#4594 = FACE_OUTER_BOUND ( 'NONE', #6531, .T. ) ;
#4595 = CARTESIAN_POINT ( 'NONE',  ( -39.99999999999999289, 0.000000000000000000, -34.99999999999997868 ) ) ;
#4596 = ORIENTED_EDGE ( 'NONE', *, *, #8365, .F. ) ;
#4597 = CARTESIAN_POINT ( 'NONE',  ( 25.99999999999998224, 8.000000000000000000, -32.99999999999999289 ) ) ;
#4598 = CARTESIAN_POINT ( 'NONE',  ( 394.0000000000001137, 240.7889724647196488, -104.2090657433598011 ) ) ;
#4599 = CARTESIAN_POINT ( 'NONE',  ( -34.99999999999996447, 0.000000000000000000, 40.00000000000000711 ) ) ;
#4600 = FACE_OUTER_BOUND ( 'NONE', #5864, .T. ) ;
#4602 = ORIENTED_EDGE ( 'NONE', *, *, #1199, .T. ) ;
#4601 = ORIENTED_EDGE ( 'NONE', *, *, #4037, .T. ) ;
#4603 = AXIS2_PLACEMENT_3D ( 'NONE', #10115, #16635, #3590 ) ;
#4604 = CARTESIAN_POINT ( 'NONE',  ( 2.844883903241205214, 40.02776846313489045, 9.064373830433188672 ) ) ;
#4605 = EDGE_CURVE ( 'NONE', #5350, #13943, #14511, .T. ) ;
#4606 = FILL_AREA_STYLE ('',( #3245 ) ) ;
#4607 = DIRECTION ( 'NONE',  ( 1.000000000000000000, 0.000000000000000000, 0.000000000000000000 ) ) ;
#4608 = DIRECTION ( 'NONE',  ( -1.000000000000000000, 0.000000000000000000, 0.000000000000000000 ) ) ;
#4609 = VERTEX_POINT ( 'NONE', #2824 ) ;
#4610 = CARTESIAN_POINT ( 'NONE',  ( -18.00000000000000711, 0.000000000000000000, 0.000000000000000000 ) ) ;
#4611 = CARTESIAN_POINT ( 'NONE',  ( 54.99999999999999289, 515.4878487013597805, -546.7230258972048205 ) ) ;
#4612 = ORIENTED_EDGE ( 'NONE', *, *, #3207, .T. ) ;
#4613 = FACE_OUTER_BOUND ( 'NONE', #6757, .T. ) ;
#4614 = CARTESIAN_POINT ( 'NONE',  ( 0.01917172636759711599, 193.2913228521273368, 37.48263776190561458 ) ) ;
#4615 = DIRECTION ( 'NONE',  ( 0.000000000000000000, 1.000000000000000000, 0.000000000000000000 ) ) ;
#4616 = FACE_OUTER_BOUND ( 'NONE', #13939, .T. ) ;
#4617 = DIRECTION ( 'NONE',  ( 1.000000000000000000, 0.000000000000000000, 0.000000000000000000 ) ) ;
#4618 = EDGE_LOOP ( 'NONE', ( #5595, #2978 ) ) ;
#4619 = DIRECTION ( 'NONE',  ( 0.000000000000000000, 0.6468954956981579629, -0.7625786632508376739 ) ) ;
#4620 = LINE ( 'NONE', #16469, #12599 ) ;
#4621 = EDGE_LOOP ( 'NONE', ( #16042, #3729, #7588, #3144, #6974, #8590, #6421, #4492, #16854, #2631, #14538, #14321, #82, #5685, #15113, #11003 ) ) ;
#4622 = VECTOR ( 'NONE', #6950, 1000.000000000000000 ) ;
#4623 = LINE ( 'NONE', #15197, #11051 ) ;
#4624 = ORIENTED_EDGE ( 'NONE', *, *, #8992, .T. ) ;
#4625 = LINE ( 'NONE', #15281, #7729 ) ;
#4626 = CARTESIAN_POINT ( 'NONE',  ( 10.00000000000000000, 372.8685141053778693, -83.18019484660869978 ) ) ;
#4627 = ORIENTED_EDGE ( 'NONE', *, *, #5257, .T. ) ;
#4628 = CARTESIAN_POINT ( 'NONE',  ( 3.850000000000000089, 0.000000000000000000, 0.000000000000000000 ) ) ;
#4629 = CARTESIAN_POINT ( 'NONE',  ( 55.99999999999989342, 493.2350855268086320, -521.8755148539809170 ) ) ;
#4630 = ORIENTED_EDGE ( 'NONE', *, *, #553, .F. ) ;
#4631 = ORIENTED_EDGE ( 'NONE', *, *, #1323, .F. ) ;
#4632 = VERTEX_POINT ( 'NONE', #9273 ) ;
#4633 = CARTESIAN_POINT ( 'NONE',  ( 394.0000000000001137, 339.1725919290087745, -16.41886574335978821 ) ) ;
#4634 = CARTESIAN_POINT ( 'NONE',  ( 2.999999999999996891, 60.00000000000000711, 9.013878188659974811 ) ) ;
#4635 = ORIENTED_EDGE ( 'NONE', *, *, #6528, .T. ) ;
#4636 = ADVANCED_FACE ( 'NONE', ( #1455 ), #6706, .T. ) ;
#4637 = EDGE_CURVE ( 'NONE', #6773, #742, #6684, .T. ) ;
#4638 = DIRECTION ( 'NONE',  ( 1.000000000000000000, 0.000000000000000000, 0.000000000000000000 ) ) ;
#4639 = CARTESIAN_POINT ( 'NONE',  ( 10.00000000000000000, 372.8685141053783241, -146.8198051533979935 ) ) ;
#4640 = ORIENTED_EDGE ( 'NONE', *, *, #11099, .T. ) ;
#4641 = DIRECTION ( 'NONE',  ( 0.000000000000000000, 0.000000000000000000, -1.000000000000000000 ) ) ;
#4642 = CARTESIAN_POINT ( 'NONE',  ( 35.00000000000003553, -20.00000000000000000, -20.99999999999999645 ) ) ;
#4643 = ORIENTED_EDGE ( 'NONE', *, *, #1765, .T. ) ;
#4644 = ADVANCED_FACE ( 'NONE', ( #14942 ), #10039, .F. ) ;
#4645 = AXIS2_PLACEMENT_3D ( 'NONE', #6771, #1711, #5743 ) ;
#4646 = ORIENTED_EDGE ( 'NONE', *, *, #2225, .T. ) ;
#4647 = ORIENTED_EDGE ( 'NONE', *, *, #8562, .F. ) ;
#4648 = ORIENTED_EDGE ( 'NONE', *, *, #8109, .T. ) ;
#4649 = SHAPE_REPRESENTATION_RELATIONSHIP ( 'NONE' , 'NONE' ,  #15920, #5866 ) ;
#4650 = ORIENTED_EDGE ( 'NONE', *, *, #477, .T. ) ;
#4651 = AXIS2_PLACEMENT_3D ( 'NONE', #9167, #2375, #2630 ) ;
#4652 = VERTEX_POINT ( 'NONE', #1880 ) ;
#4653 = FACE_OUTER_BOUND ( 'NONE', #12982, .T. ) ;
#4654 = EDGE_CURVE ( 'NONE', #7744, #12451, #5622, .T. ) ;
#4655 = AXIS2_PLACEMENT_3D ( 'NONE', #13312, #12596, #5903 ) ;
#4656 = CARTESIAN_POINT ( 'NONE',  ( -20.00000000000003197, 3.000000000000000000, 37.00000000000000711 ) ) ;
#4657 = DIRECTION ( 'NONE',  ( 0.000000000000000000, 0.000000000000000000, -1.000000000000000000 ) ) ;
#4658 = CARTESIAN_POINT ( 'NONE',  ( 0.000000000000000000, 226.8713558223388134, -333.7582248962859808 ) ) ;
#4659 = DIRECTION ( 'NONE',  ( -1.000000000000000000, 0.000000000000000000, 0.000000000000000000 ) ) ;
#4660 = FACE_OUTER_BOUND ( 'NONE', #14218, .T. ) ;
#4661 = EDGE_CURVE ( 'NONE', #6401, #14529, #599, .T. ) ;
#4662 = EDGE_CURVE ( 'NONE', #9375, #1983, #10290, .T. ) ;
#4663 = EDGE_CURVE ( 'NONE', #13923, #5700, #14962, .T. ) ;
#4664 = CARTESIAN_POINT ( 'NONE',  ( 31.00000000000001421, 0.000000000000000000, 25.99999999999999645 ) ) ;
#4665 = EDGE_CURVE ( 'NONE', #1142, #15212, #5061, .T. ) ;
#4666 = DIRECTION ( 'NONE',  ( 0.000000000000000000, 0.000000000000000000, -1.000000000000000000 ) ) ;
#4667 = ORIENTED_EDGE ( 'NONE', *, *, #11283, .T. ) ;
#4668 = DIRECTION ( 'NONE',  ( 0.000000000000000000, 0.000000000000000000, 1.000000000000000000 ) ) ;
#4669 = FACE_OUTER_BOUND ( 'NONE', #16405, .T. ) ;
#4670 = VECTOR ( 'NONE', #4925, 1000.000000000000000 ) ;
#4671 = CARTESIAN_POINT ( 'NONE',  ( 1.250085104875786612E-12, 220.0768326692952996, 286.9685381829922903 ) ) ;
#4672 = LINE ( 'NONE', #9925, #12892 ) ;
#4674 = ORIENTED_EDGE ( 'NONE', *, *, #1441, .T. ) ;
#4673 = VERTEX_POINT ( 'NONE', #9792 ) ;
#4675 = APPLICATION_CONTEXT ( 'automotive_design' ) ;
#4676 = DIRECTION ( 'NONE',  ( 1.000000000000000000, 0.000000000000000000, -0.000000000000000000 ) ) ;
#4677 = ORIENTED_EDGE ( 'NONE', *, *, #9286, .F. ) ;
#4678 = DIRECTION ( 'NONE',  ( 0.000000000000000000, 0.000000000000000000, -1.000000000000000000 ) ) ;
#4679 = LINE ( 'NONE', #5976, #16535 ) ;
#4680 = CIRCLE ( 'NONE', #2761, 9.000000000000007105 ) ;
#4681 = ORIENTED_EDGE ( 'NONE', *, *, #16934, .F. ) ;
#4682 = UNCERTAINTY_MEASURE_WITH_UNIT (LENGTH_MEASURE( 1.000000000000000082E-05 ), #11912, 'distance_accuracy_value', 'NONE');
#4683 = DIRECTION ( 'NONE',  ( 1.000000000000000000, -0.000000000000000000, -0.000000000000000000 ) ) ;
#4684 = EDGE_CURVE ( 'NONE', #5265, #1542, #15767, .T. ) ;
#4685 = EDGE_CURVE ( 'NONE', #4809, #1870, #967, .T. ) ;
#4686 = CARTESIAN_POINT ( 'NONE',  ( 35.99999999999999289, 6.000000000000000000, 17.99999999999998934 ) ) ;
#4687 = EDGE_LOOP ( 'NONE', ( #9214, #10983, #11510, #6237 ) ) ;
#4688 = FACE_OUTER_BOUND ( 'NONE', #810, .T. ) ;
#4689 = EDGE_CURVE ( 'NONE', #15644, #4224, #10562, .T. ) ;
#4690 = CARTESIAN_POINT ( 'NONE',  ( -3.302699999997892544, 192.9602775880926515, 37.54929111636569417 ) ) ;
#4691 = DIRECTION ( 'NONE',  ( -1.000000000000000000, 0.000000000000000000, 0.000000000000000000 ) ) ;
#4692 = CARTESIAN_POINT ( 'NONE',  ( -31.00000000000005329, 10.00000000000000000, -26.00000000000000355 ) ) ;
#4693 = CYLINDRICAL_SURFACE ( 'NONE', #4603, 8.000000000000000000 ) ;
#4694 = VERTEX_POINT ( 'NONE', #1956 ) ;
#4695 = AXIS2_PLACEMENT_3D ( 'NONE', #5362, #11725, #4085 ) ;
#4696 = FACE_OUTER_BOUND ( 'NONE', #7470, .T. ) ;
#4697 = CARTESIAN_POINT ( 'NONE',  ( -36.00000000000000711, 6.000000000000000000, -22.00000000000000355 ) ) ;
#4698 = VECTOR ( 'NONE', #14687, 1000.000000000000000 ) ;
#4699 = ORIENTED_EDGE ( 'NONE', *, *, #3019, .T. ) ;
#4700 = AXIS2_PLACEMENT_3D ( 'NONE', #3768, #9082, #1092 ) ;
#4701 = ADVANCED_FACE ( 'NONE', ( #4696 ), #16310, .T. ) ;
#4702 = CARTESIAN_POINT ( 'NONE',  ( 31.00000000000002842, 68.00000000000000000, 26.00000000000001066 ) ) ;
#4703 = EDGE_LOOP ( 'NONE', ( #12505, #12097, #12154, #4953, #14764, #2405, #16340, #11690 ) ) ;
#4704 = AXIS2_PLACEMENT_3D ( 'NONE', #13433, #9383, #14878 ) ;
#4705 = CARTESIAN_POINT ( 'NONE',  ( -37.00000000000000711, 10.00000000000000000, 23.00000000000000000 ) ) ;
#4706 = ORIENTED_EDGE ( 'NONE', *, *, #11748, .F. ) ;
#4707 = CARTESIAN_POINT ( 'NONE',  ( -46.99999999999988631, 549.5810598491746077, -518.1154249974242703 ) ) ;
#4708 = LINE ( 'NONE', #5674, #14217 ) ;
#4709 = CARTESIAN_POINT ( 'NONE',  ( 56.72999999999999687, 214.4632308570087957, 287.5298983642209123 ) ) ;
#4710 = ORIENTED_EDGE ( 'NONE', *, *, #16927, .F. ) ;
#4711 = AXIS2_PLACEMENT_3D ( 'NONE', #16274, #9763, #12406 ) ;
#4712 = AXIS2_PLACEMENT_3D ( 'NONE', #14060, #7520, #149 ) ;
#4713 = CARTESIAN_POINT ( 'NONE',  ( 45.00000000000000000, 473.6663340069158039, -575.6402177818052905 ) ) ;
#4714 = VECTOR ( 'NONE', #2963, 1000.000000000000000 ) ;
#4715 = CARTESIAN_POINT ( 'NONE',  ( -55.99999999999989342, 523.2161522479893847, -590.5524132976893270 ) ) ;
#4716 = ORIENTED_EDGE ( 'NONE', *, *, #1993, .T. ) ;
#4717 = ORIENTED_EDGE ( 'NONE', *, *, #14408, .F. ) ;
#4718 = DIRECTION ( 'NONE',  ( -0.000000000000000000, 0.000000000000000000, 1.000000000000000000 ) ) ;
#4719 = PRODUCT_CONTEXT ( 'NONE', #7082, 'mechanical' ) ;
#4720 = CIRCLE ( 'NONE', #6089, 59.99999999999994316 ) ;
#4721 = CARTESIAN_POINT ( 'NONE',  ( 2.259918635623968441, 61.98265998586796854, 9.228371864727256124 ) ) ;
#4722 = ORIENTED_EDGE ( 'NONE', *, *, #5842, .T. ) ;
#4723 = MECHANICAL_DESIGN_GEOMETRIC_PRESENTATION_REPRESENTATION (  '', ( #14618 ), #16798 ) ;
#4724 = DIRECTION ( 'NONE',  ( 0.000000000000000000, 0.000000000000000000, -1.000000000000000000 ) ) ;
#4725 = CARTESIAN_POINT ( 'NONE',  ( 7.000000000000000000, 0.000000000000000000, 0.000000000000000000 ) ) ;
#4726 = ORIENTED_EDGE ( 'NONE', *, *, #11407, .T. ) ;
#4727 = DIRECTION ( 'NONE',  ( 1.049727191138612163E-16, 0.5150380749100629263, -0.8571673007021070045 ) ) ;
#4728 = LINE ( 'NONE', #8523, #5645 ) ;
#4729 = VERTEX_POINT ( 'NONE', #12441 ) ;
#4730 = DIRECTION ( 'NONE',  ( 0.000000000000000000, 0.000000000000000000, -1.000000000000000000 ) ) ;
#4731 = EDGE_LOOP ( 'NONE', ( #13958, #8713, #2598, #8250 ) ) ;
#4732 = ORIENTED_EDGE ( 'NONE', *, *, #6292, .F. ) ;
#4733 = EDGE_CURVE ( 'NONE', #4278, #12140, #12524, .T. ) ;
#4734 = VECTOR ( 'NONE', #385, 1000.000000000000000 ) ;
#4735 = AXIS2_PLACEMENT_3D ( 'NONE', #16454, #11053, #2026 ) ;
#4736 = VERTEX_POINT ( 'NONE', #8578 ) ;
#4737 =( LENGTH_UNIT ( ) NAMED_UNIT ( * ) SI_UNIT ( .MILLI., .METRE. ) );
#4738 = VERTEX_POINT ( 'NONE', #16219 ) ;
#4739 = CIRCLE ( 'NONE', #2826, 34.00000000000000000 ) ;
#4740 = ADVANCED_FACE ( 'NONE', ( #683 ), #3179, .T. ) ;
#4741 = EDGE_LOOP ( 'NONE', ( #11225, #4025, #7198, #2525 ) ) ;
#4742 = FACE_OUTER_BOUND ( 'NONE', #14114, .T. ) ;
#4743 = CARTESIAN_POINT ( 'NONE',  ( -49.99999999999999289, 515.4878487013597805, -546.7230258972048205 ) ) ;
#4744 = DIRECTION ( 'NONE',  ( 0.000000000000000000, 1.000000000000000000, -0.000000000000000000 ) ) ;
#4745 = COLOUR_RGB ( '', 0.09019608, 0.27058824, 0.51372549) ;
#4746 = CIRCLE ( 'NONE', #7209, 17.52499999999999858 ) ;
#4747 = PLANE ( 'NONE',  #1603 ) ;
#4748 = CARTESIAN_POINT ( 'NONE',  ( 0.7366000000000156867, 214.4632308570090800, 287.5298983642209691 ) ) ;
#4749 = VECTOR ( 'NONE', #3303, 1000.000000000000000 ) ;
#4750 = CARTESIAN_POINT ( 'NONE',  ( 10.00000000000000000, 336.2713855965630501, -311.0652884549417081 ) ) ;
#4751 = DIRECTION ( 'NONE',  ( 2.556703065963791256E-16, -1.000000000000000000, 0.000000000000000000 ) ) ;
#4752 = FACE_BOUND ( 'NONE', #9265, .T. ) ;
#4753 = ORIENTED_EDGE ( 'NONE', *, *, #1204, .T. ) ;
#4754 = DIRECTION ( 'NONE',  ( 0.000000000000000000, 0.000000000000000000, 1.000000000000000000 ) ) ;
#4755 = DIRECTION ( 'NONE',  ( 0.000000000000000000, -0.000000000000000000, 1.000000000000000000 ) ) ;
#4756 = CIRCLE ( 'NONE', #14086, 4.999999999999997335 ) ;
#4757 = EDGE_CURVE ( 'NONE', #4921, #1899, #9749, .T. ) ;
#4758 = EDGE_CURVE ( 'NONE', #14998, #11320, #2604, .T. ) ;
#4759 = LINE ( 'NONE', #1863, #5477 ) ;
#4761 = ORIENTED_EDGE ( 'NONE', *, *, #1526, .F. ) ;
#4760 = VERTEX_POINT ( 'NONE', #4455 ) ;
#4762 = AXIS2_PLACEMENT_3D ( 'NONE', #16258, #11264, #5775 ) ;
#4763 = DIRECTION ( 'NONE',  ( 0.000000000000000000, 0.000000000000000000, 1.000000000000000000 ) ) ;
#4764 = VECTOR ( 'NONE', #14535, 1000.000000000000000 ) ;
#4765 = ORIENTED_EDGE ( 'NONE', *, *, #2784, .F. ) ;
#4766 = EDGE_CURVE ( 'NONE', #478, #5489, #13573, .T. ) ;
#4767 = EDGE_CURVE ( 'NONE', #785, #2908, #4528, .T. ) ;
#4768 = CARTESIAN_POINT ( 'NONE',  ( -34.99999999999996447, 0.000000000000000000, 40.00000000000000711 ) ) ;
#4769 = ADVANCED_FACE ( 'NONE', ( #12357 ), #7433, .F. ) ;
#4770 = VECTOR ( 'NONE', #3630, 1000.000000000000000 ) ;
#4771 = DIRECTION ( 'NONE',  ( -1.000000000000000000, 0.000000000000000000, -0.000000000000000000 ) ) ;
#4772 = DIRECTION ( 'NONE',  ( 0.000000000000000000, 0.000000000000000000, 1.000000000000000000 ) ) ;
#4773 = AXIS2_PLACEMENT_3D ( 'NONE', #9365, #2838, #16150 ) ;
#4774 = ORIENTED_EDGE ( 'NONE', *, *, #5956, .F. ) ;
#4775 = CARTESIAN_POINT ( 'NONE',  ( -20.00000000000003197, 3.000000000000000000, 37.00000000000000711 ) ) ;
#4776 =( GEOMETRIC_REPRESENTATION_CONTEXT ( 3 ) GLOBAL_UNCERTAINTY_ASSIGNED_CONTEXT ( ( #15799 ) ) GLOBAL_UNIT_ASSIGNED_CONTEXT ( ( #391, #1843, #12565 ) ) REPRESENTATION_CONTEXT ( 'NONE', 'WORKASPACE' ) );
#4777 = CARTESIAN_POINT ( 'NONE',  ( 0.07938566280257335073, 193.0939377745695822, 37.43526655022207450 ) ) ;
#4778 = ORIENTED_EDGE ( 'NONE', *, *, #14433, .F. ) ;
#4779 = PLANE ( 'NONE',  #10428 ) ;
#4780 = AXIS2_PLACEMENT_3D ( 'NONE', #13111, #12847, #3755 ) ;
#4781 = APPLICATION_CONTEXT ( 'automotive_design' ) ;
#4782 = CARTESIAN_POINT ( 'NONE',  ( 0.000000000000000000, 341.5974953295086038, -15.94751227074151956 ) ) ;
#4783 = CARTESIAN_POINT ( 'NONE',  ( 10.00000000000000000, 301.0487089519837127, -150.0000000000038369 ) ) ;
#4784 = EDGE_CURVE ( 'NONE', #10898, #13853, #5034, .T. ) ;
#4785 = LINE ( 'NONE', #7351, #5453 ) ;
#4786 = CARTESIAN_POINT ( 'NONE',  ( -25.99999999999999645, 0.000000000000000000, -31.00000000000003197 ) ) ;
#4787 = ORIENTED_EDGE ( 'NONE', *, *, #5809, .F. ) ;
#4788 = DIRECTION ( 'NONE',  ( 0.000000000000000000, 0.000000000000000000, 1.000000000000000000 ) ) ;
#4789 = EDGE_CURVE ( 'NONE', #2788, #6952, #3839, .T. ) ;
#4790 = EDGE_CURVE ( 'NONE', #14343, #9226, #7774, .T. ) ;
#4791 = EDGE_CURVE ( 'NONE', #8452, #11485, #11403, .T. ) ;
#4792 = FACE_OUTER_BOUND ( 'NONE', #10269, .T. ) ;
#4793 = EDGE_CURVE ( 'NONE', #12485, #3376, #10375, .T. ) ;
#4794 = ORIENTED_EDGE ( 'NONE', *, *, #3297, .T. ) ;
#4795 = CARTESIAN_POINT ( 'NONE',  ( 3.500000000000000000, 14.59999999999999964, 0.000000000000000000 ) ) ;
#4796 = ORIENTED_EDGE ( 'NONE', *, *, #2921, .T. ) ;
#4797 = CIRCLE ( 'NONE', #425, 17.85000000000000142 ) ;
#4798 = DIRECTION ( 'NONE',  ( 1.000000000000000000, 0.000000000000000000, 0.000000000000000000 ) ) ;
#4799 = AXIS2_PLACEMENT_3D ( 'NONE', #1878, #8918, #12854 ) ;
#4800 = FACE_OUTER_BOUND ( 'NONE', #16420, .T. ) ;
#4801 = ORIENTED_EDGE ( 'NONE', *, *, #5632, .T. ) ;
#4802 = LINE ( 'NONE', #13830, #14381 ) ;
#4803 = LINE ( 'NONE', #6321, #798 ) ;
#4804 = DIRECTION ( 'NONE',  ( -0.000000000000000000, 1.000000000000000000, -0.000000000000000000 ) ) ;
#4805 = ORIENTED_EDGE ( 'NONE', *, *, #12273, .F. ) ;
#4806 = SURFACE_SIDE_STYLE ('',( #2221 ) ) ;
#4807 = CARTESIAN_POINT ( 'NONE',  ( 35.00000000000000711, 8.000000000000000000, 20.99999999999999289 ) ) ;
#4808 = DIRECTION ( 'NONE',  ( -0.000000000000000000, 0.09950371902099770793, -0.9950371902099891530 ) ) ;
#4809 = VERTEX_POINT ( 'NONE', #2295 ) ;
#4810 = VERTEX_POINT ( 'NONE', #11560 ) ;
#4811 = CARTESIAN_POINT ( 'NONE',  ( 31.00000000000003553, 19.00000000000000000, 20.99999999999999289 ) ) ;
#4812 = VECTOR ( 'NONE', #3592, 1000.000000000000000 ) ;
#4813 = APPLICATION_PROTOCOL_DEFINITION ( 'draft international standard', 'automotive_design', 1998, #16736 ) ;
#4814 = DIRECTION ( 'NONE',  ( 1.000000000000000000, -0.000000000000000000, 0.000000000000000000 ) ) ;
#4815 = ORIENTED_EDGE ( 'NONE', *, *, #15609, .F. ) ;
#4816 = FACE_OUTER_BOUND ( 'NONE', #13136, .T. ) ;
#4817 = CARTESIAN_POINT ( 'NONE',  ( -31.81980515339462912, 8.000000000000000000, -28.51980515339464972 ) ) ;
#4818 = ORIENTED_EDGE ( 'NONE', *, *, #7072, .T. ) ;
#4819 = VECTOR ( 'NONE', #4763, 1000.000000000000000 ) ;
#4820 = CYLINDRICAL_SURFACE ( 'NONE', #103, 22.75209553982837463 ) ;
#4821 = DIRECTION ( 'NONE',  ( -0.000000000000000000, -1.000000000000000000, -0.000000000000000000 ) ) ;
#4822 = VERTEX_POINT ( 'NONE', #12859 ) ;
#4823 = DIRECTION ( 'NONE',  ( -0.000000000000000000, -1.000000000000000000, -0.000000000000000000 ) ) ;
#4824 = ADVANCED_FACE ( 'NONE', ( #4871 ), #1091, .T. ) ;
#4825 = ORIENTED_EDGE ( 'NONE', *, *, #15868, .F. ) ;
#4826 = ORIENTED_EDGE ( 'NONE', *, *, #8155, .T. ) ;
#4827 = ORIENTED_EDGE ( 'NONE', *, *, #7860, .F. ) ;
#4828 =( LENGTH_UNIT ( ) NAMED_UNIT ( * ) SI_UNIT ( .MILLI., .METRE. ) );
#4829 = VECTOR ( 'NONE', #5753, 1000.000000000000000 ) ;
#4830 = EDGE_CURVE ( 'NONE', #11889, #2294, #6394, .T. ) ;
#4831 = AXIS2_PLACEMENT_3D ( 'NONE', #11322, #7191, #12450 ) ;
#4832 = ORIENTED_EDGE ( 'NONE', *, *, #4535, .T. ) ;
#4833 = ORIENTED_EDGE ( 'NONE', *, *, #14333, .T. ) ;
#4834 = CYLINDRICAL_SURFACE ( 'NONE', #1435, 4.999999999999997335 ) ;
#4835 = CARTESIAN_POINT ( 'NONE',  ( -39.99999999999999289, 11.00000000000000000, -26.00000000000000355 ) ) ;
#4836 = LINE ( 'NONE', #2340, #10518 ) ;
#4837 = PRODUCT_DEFINITION ( 'UNKNOWN', '', #1218, #7422 ) ;
#4838 = DIRECTION ( 'NONE',  ( -1.000000000000000000, -0.000000000000000000, -0.000000000000000000 ) ) ;
#4839 = CARTESIAN_POINT ( 'NONE',  ( -2.220446049250313081E-13, 75.00000000000001421, 0.000000000000000000 ) ) ;
#4840 = FACE_OUTER_BOUND ( 'NONE', #2027, .T. ) ;
#4841 = VECTOR ( 'NONE', #15932, 1000.000000000000000 ) ;
#4842 = CARTESIAN_POINT ( 'NONE',  ( -23.00000000000002132, 6.000000000000000000, 37.00000000000000711 ) ) ;
#4843 = AXIS2_PLACEMENT_3D ( 'NONE', #9229, #9134, #7834 ) ;
#4844 = CARTESIAN_POINT ( 'NONE',  ( -46.99999999999988631, 493.2350855268092573, -585.2659423243250103 ) ) ;
#4845 = ORIENTED_EDGE ( 'NONE', *, *, #4993, .F. ) ;
#4846 = CARTESIAN_POINT ( 'NONE',  ( 1.050000000000000044, 0.000000000000000000, 0.000000000000000000 ) ) ;
#4847 = DIRECTION ( 'NONE',  ( 0.000000000000000000, -0.000000000000000000, 1.000000000000000000 ) ) ;
#4848 = EDGE_CURVE ( 'NONE', #15887, #15487, #10298, .T. ) ;
#4849 = DIRECTION ( 'NONE',  ( -1.000000000000000000, -0.000000000000000000, -0.000000000000000000 ) ) ;
#4851 = ORIENTED_EDGE ( 'NONE', *, *, #13718, .T. ) ;
#4850 = ORIENTED_EDGE ( 'NONE', *, *, #15396, .F. ) ;
#4852 = DIRECTION ( 'NONE',  ( 0.000000000000000000, 0.000000000000000000, 1.000000000000000000 ) ) ;
#4853 = VERTEX_POINT ( 'NONE', #16796 ) ;
#4854 = VECTOR ( 'NONE', #16089, 1000.000000000000000 ) ;
#4855 = SURFACE_STYLE_USAGE ( .BOTH. , #14390 ) ;
#4856 = FACE_OUTER_BOUND ( 'NONE', #703, .T. ) ;
#4857 = CARTESIAN_POINT ( 'NONE',  ( 39.99999999999999289, 10.00000000000000000, 26.00000000000000000 ) ) ;
#4858 = VERTEX_POINT ( 'NONE', #1017 ) ;
#4859 = EDGE_CURVE ( 'NONE', #1879, #2075, #12782, .T. ) ;
#4860 = PRODUCT_DEFINITION_CONTEXT ( 'detailed design', #4675, 'design' ) ;
#4861 = DIRECTION ( 'NONE',  ( 0.000000000000000000, 0.000000000000000000, -1.000000000000000000 ) ) ;
#4862 = DIRECTION ( 'NONE',  ( 0.000000000000000000, 0.000000000000000000, -1.000000000000000000 ) ) ;
#4863 = ORIENTED_EDGE ( 'NONE', *, *, #9959, .F. ) ;
#4864 = CYLINDRICAL_SURFACE ( 'NONE', #10125, 3.000000000000002665 ) ;
#4865 = CARTESIAN_POINT ( 'NONE',  ( 0.3822672831244716130, 192.8515144050814456, 37.32528944829227413 ) ) ;
#4866 = CARTESIAN_POINT ( 'NONE',  ( -35.00000000000000000, 8.000000000000000000, -21.00000000000000000 ) ) ;
#4867 = EDGE_CURVE ( 'NONE', #11960, #10491, #15353, .T. ) ;
#4868 = CARTESIAN_POINT ( 'NONE',  ( -55.99999999999988631, 334.9272574771864015, -321.9943432880672276 ) ) ;
#4869 = CYLINDRICAL_SURFACE ( 'NONE', #7336, 4.999999999999997335 ) ;
#4870 = ORIENTED_EDGE ( 'NONE', *, *, #3967, .T. ) ;
#4871 = FACE_OUTER_BOUND ( 'NONE', #13857, .T. ) ;
#4872 = DIRECTION ( 'NONE',  ( 0.000000000000000000, 1.000000000000000000, 0.000000000000000000 ) ) ;
#4873 = CARTESIAN_POINT ( 'NONE',  ( 0.000000000000000000, 620.7506394335853201, 305.2562418976663707 ) ) ;
#4874 = TOROIDAL_SURFACE ( 'NONE', #7886, 4.695405383895982609, 9.000000000000000000 ) ;
#4875 = ORIENTED_EDGE ( 'NONE', *, *, #10985, .F. ) ;
#4876 = EDGE_CURVE ( 'NONE', #9661, #12229, #8098, .T. ) ;
#4877 = AXIS2_PLACEMENT_3D ( 'NONE', #14788, #9460, #2749 ) ;
#4878 = CARTESIAN_POINT ( 'NONE',  ( 1.399999999999999911, -15.25000000000000000, -1.867586368699713770E-15 ) ) ;
#4879 = LINE ( 'NONE', #8928, #4021 ) ;
#4880 = EDGE_LOOP ( 'NONE', ( #14735, #12528, #2019, #13484 ) ) ;
#4881 = CYLINDRICAL_SURFACE ( 'NONE', #4233, 13.69540538389601991 ) ;
#4882 = EDGE_CURVE ( 'NONE', #10633, #16779, #11655, .T. ) ;
#4883 = CARTESIAN_POINT ( 'NONE',  ( 75.00000000000000000, 277.8092731128509740, -44.71049682360897748 ) ) ;
#4884 = CARTESIAN_POINT ( 'NONE',  ( 10.00000000000000000, 372.8685141053783241, -146.8198051533979935 ) ) ;
#4885 = ORIENTED_EDGE ( 'NONE', *, *, #8653, .T. ) ;
#4886 = EDGE_CURVE ( 'NONE', #14448, #9650, #6482, .T. ) ;
#4887 = EDGE_CURVE ( 'NONE', #12156, #5336, #4947, .T. ) ;
#4888 = ADVANCED_FACE ( 'NONE', ( #13982 ), #6233, .F. ) ;
#4889 = DIRECTION ( 'NONE',  ( -0.000000000000000000, -1.000000000000000000, -0.000000000000000000 ) ) ;
#4890 = CARTESIAN_POINT ( 'NONE',  ( 45.00000000000000000, 523.2161522479888163, -516.5890438806160319 ) ) ;
#4891 = CARTESIAN_POINT ( 'NONE',  ( 0.000000000000000000, 0.000000000000000000, -11.00000000000000000 ) ) ;
#4892 = ORIENTED_EDGE ( 'NONE', *, *, #9225, .T. ) ;
#4893 = DIRECTION ( 'NONE',  ( -0.000000000000000000, -1.000000000000000000, -0.000000000000000000 ) ) ;
#4894 = AXIS2_PLACEMENT_3D ( 'NONE', #568, #12076, #5714 ) ;
#4895 = ITEM_DEFINED_TRANSFORMATION ( 'NONE', 'NONE', #14115,  #1488 ) ;
#4896 = LINE ( 'NONE', #14578, #4949 ) ;
#4897 = VERTEX_POINT ( 'NONE', #15435 ) ;
#4898 = LINE ( 'NONE', #2402, #15417 ) ;
#4899 = CARTESIAN_POINT ( 'NONE',  ( -13.11912225705329327, 0.000000000000000000, 22.50000000000000000 ) ) ;
#4900 = EDGE_LOOP ( 'NONE', ( #3063, #16869, #15004, #13150, #1047 ) ) ;
#4901 = LINE ( 'NONE', #627, #934 ) ;
#4902 = LINE ( 'NONE', #2239, #10860 ) ;
#4903 = ORIENTED_EDGE ( 'NONE', *, *, #5035, .T. ) ;
#4904 = EDGE_CURVE ( 'NONE', #7594, #14585, #8748, .T. ) ;
#4905 = DIRECTION ( 'NONE',  ( -1.000000000000000000, -0.000000000000000000, -0.000000000000000000 ) ) ;
#4906 = EDGE_LOOP ( 'NONE', ( #10943, #4825, #8516, #2285 ) ) ;
#4907 = ORIENTED_EDGE ( 'NONE', *, *, #10062, .T. ) ;
#4908 = VERTEX_POINT ( 'NONE', #3680 ) ;
#4909 =( NAMED_UNIT ( * ) PLANE_ANGLE_UNIT ( ) SI_UNIT ( $, .RADIAN. ) );
#4910 = PRODUCT ( 'Servo-Head', 'Servo-Head', '', ( #15300 ) ) ;
#4911 = ORIENTED_EDGE ( 'NONE', *, *, #11307, .T. ) ;
#4912 = VERTEX_POINT ( 'NONE', #8921 ) ;
#4913 = DIRECTION ( 'NONE',  ( -0.000000000000000000, 1.000000000000000000, -0.000000000000000000 ) ) ;
#4914 = CARTESIAN_POINT ( 'NONE',  ( 10.00000000000000000, 202.9739201934855828, -514.2167050642598269 ) ) ;
#4915 = CIRCLE ( 'NONE', #3003, 13.95000000000000107 ) ;
#4916 = CARTESIAN_POINT ( 'NONE',  ( -32.00000000000000711, 6.000000000000000000, -22.00000000000000355 ) ) ;
#4917 = DIRECTION ( 'NONE',  ( 1.000000000000000000, 0.000000000000000000, 0.000000000000000000 ) ) ;
#4918 = DIRECTION ( 'NONE',  ( 0.000000000000000000, 0.000000000000000000, -1.000000000000000000 ) ) ;
#4919 = DIRECTION ( 'NONE',  ( -1.000000000000000000, -0.000000000000000000, -0.000000000000000000 ) ) ;
#4920 = FACE_OUTER_BOUND ( 'NONE', #5568, .T. ) ;
#4921 = VERTEX_POINT ( 'NONE', #15682 ) ;
#4922 = DIRECTION ( 'NONE',  ( 0.000000000000000000, -1.000000000000000000, 0.000000000000000000 ) ) ;
#4923 = CARTESIAN_POINT ( 'NONE',  ( 5.425003271131650706, -12.64814671169700055, 1.549064719741994274E-15 ) ) ;
#4924 = VERTEX_POINT ( 'NONE', #11916 ) ;
#4925 = DIRECTION ( 'NONE',  ( -0.000000000000000000, -1.000000000000000000, -0.000000000000000000 ) ) ;
#4927 = ORIENTED_EDGE ( 'NONE', *, *, #16170, .F. ) ;
#4926 = ORIENTED_EDGE ( 'NONE', *, *, #15504, .F. ) ;
#4928 = CARTESIAN_POINT ( 'NONE',  ( 17.99999999999998224, 6.000000000000000000, -35.99999999999999289 ) ) ;
#4929 = TOROIDAL_SURFACE ( 'NONE', #14268, 4.695405383895982609, 9.000000000000000000 ) ;
#4930 = AXIS2_PLACEMENT_3D ( 'NONE', #14586, #2815, #8054 ) ;
#4931 = DIRECTION ( 'NONE',  ( -1.000000000000000000, 0.000000000000000000, -0.000000000000000000 ) ) ;
#4932 = AXIS2_PLACEMENT_3D ( 'NONE', #2472, #12956, #7449 ) ;
#4933 = CARTESIAN_POINT ( 'NONE',  ( 415.0210210471910841, 329.6061121441327941, -6.736600000000000144 ) ) ;
#4934 = CARTESIAN_POINT ( 'NONE',  ( 22.99999999999995737, 0.000000000000000000, -36.99999999999999289 ) ) ;
#4935 = EDGE_LOOP ( 'NONE', ( #8859, #14753, #4319, #6458, #11809, #11446, #4926, #3819 ) ) ;
#4936 = CARTESIAN_POINT ( 'NONE',  ( 31.81980515339464333, 8.000000000000000000, 28.51980515339463906 ) ) ;
#4937 = CIRCLE ( 'NONE', #16193, 2.999999999999995559 ) ;
#4938 = CARTESIAN_POINT ( 'NONE',  ( 394.0000000000001137, 240.7889724647196488, -104.2090657433598011 ) ) ;
#4939 = ORIENTED_EDGE ( 'NONE', *, *, #16737, .T. ) ;
#4940 = CARTESIAN_POINT ( 'NONE',  ( 55.99999999999989342, 549.5810598491746077, -522.8108303813202156 ) ) ;
#4941 = VECTOR ( 'NONE', #2626, 1000.000000000000000 ) ;
#4942 = CARTESIAN_POINT ( 'NONE',  ( -9.000000000000001776, 0.000000000000000000, 0.000000000000000000 ) ) ;
#4943 = LINE ( 'NONE', #15523, #15138 ) ;
#4944 = DIRECTION ( 'NONE',  ( 0.000000000000000000, 0.000000000000000000, 1.000000000000000000 ) ) ;
#4945 = DIRECTION ( 'NONE',  ( 0.000000000000000000, 0.000000000000000000, -1.000000000000000000 ) ) ;
#4946 = EDGE_LOOP ( 'NONE', ( #11020, #16073, #15657, #2337 ) ) ;
#4947 = LINE ( 'NONE', #13589, #13324 ) ;
#4948 = EDGE_CURVE ( 'NONE', #12146, #14019, #4279, .T. ) ;
#4949 = VECTOR ( 'NONE', #14091, 1000.000000000000000 ) ;
#4950 = PLANE ( 'NONE',  #6329 ) ;
#4951 = LINE ( 'NONE', #2382, #11606 ) ;
#4952 = EDGE_CURVE ( 'NONE', #10385, #7889, #4184, .T. ) ;
#4953 = ORIENTED_EDGE ( 'NONE', *, *, #11273, .T. ) ;
#4954 = FACE_OUTER_BOUND ( 'NONE', #7585, .T. ) ;
#4955 = DIRECTION ( 'NONE',  ( 0.000000000000000000, 0.000000000000000000, -1.000000000000000000 ) ) ;
#4956 = ORIENTED_EDGE ( 'NONE', *, *, #5935, .F. ) ;
#4957 = DIRECTION ( 'NONE',  ( -6.123031769111888756E-17, 1.000000000000000000, 3.749151804555344967E-33 ) ) ;
#4958 = CARTESIAN_POINT ( 'NONE',  ( -22.00000000000001776, 6.000000000000000000, 36.00000000000000711 ) ) ;
#4959 = LINE ( 'NONE', #15453, #12783 ) ;
#4960 = ORIENTED_EDGE ( 'NONE', *, *, #2791, .F. ) ;
#4961 = AXIS2_PLACEMENT_3D ( 'NONE', #15515, #8986, #2705 ) ;
#4962 = DIRECTION ( 'NONE',  ( 1.000000000000000000, -0.000000000000000000, -0.000000000000000000 ) ) ;
#4963 = LINE ( 'NONE', #4807, #10622 ) ;
#4964 = CARTESIAN_POINT ( 'NONE',  ( -1.725642888253134277, 288.6479481343113207, 37.61614439054953607 ) ) ;
#4965 = ORIENTED_EDGE ( 'NONE', *, *, #9411, .F. ) ;
#4966 = LINE ( 'NONE', #11425, #7238 ) ;
#4967 = EDGE_CURVE ( 'NONE', #4486, #13331, #7544, .T. ) ;
#4968 = CLOSED_SHELL ( 'NONE', ( #12804, #7182, #14843, #12480, #6095, #665, #15042, #14965, #595, #5629, #11135, #14427, #9521, #9735, #4769, #5953, #12396, #16444, #3533, #16812, #11427, #14616, #8584, #14199, #9347, #12942, #2586, #13401, #12975, #12004, #12434, #9906, #321, #9296, #3724, #14765, #3448, #1912, #751, #1543, #2125, #16559, #2678, #14238, #6045, #13276, #10556, #14127, #1764, #6042, #13002, #482, #14657, #3611, #13669, #13905, #15261, #10038, #6759, #16764, #9496, #694, #6003, #13388, #7367, #6019 ) ) ;
#4969 = EDGE_CURVE ( 'NONE', #14523, #1188, #14671, .T. ) ;
#4970 = VECTOR ( 'NONE', #13930, 1000.000000000000000 ) ;
#4971 = ADVANCED_FACE ( 'NONE', ( #6568 ), #13862, .T. ) ;
#4972 = ORIENTED_EDGE ( 'NONE', *, *, #4155, .T. ) ;
#4973 = EDGE_CURVE ( 'NONE', #14275, #8711, #5358, .T. ) ;
#4974 = CARTESIAN_POINT ( 'NONE',  ( -39.99999999999999289, 8.000000000000000000, -34.99999999999997868 ) ) ;
#4975 = DIRECTION ( 'NONE',  ( 0.000000000000000000, 0.000000000000000000, -1.000000000000000000 ) ) ;
#4976 = CARTESIAN_POINT ( 'NONE',  ( 22.99999999999998224, 0.000000000000000000, 37.00000000000000711 ) ) ;
#4977 = EDGE_LOOP ( 'NONE', ( #12366, #7904, #8961, #5215 ) ) ;
#4978 = DIRECTION ( 'NONE',  ( 0.000000000000000000, -0.8660254037844379305, -0.5000000000000012212 ) ) ;
#4979 = PRESENTATION_LAYER_ASSIGNMENT (  '', '', ( #14041 ) ) ;
#4980 = CARTESIAN_POINT ( 'NONE',  ( -36.00000000000000711, 8.000000000000000000, -22.00000000000000355 ) ) ;
#4981 = VERTEX_POINT ( 'NONE', #2633 ) ;
#4982 = CYLINDRICAL_SURFACE ( 'NONE', #3403, 13.69540538389601991 ) ;
#4983 = ORIENTED_EDGE ( 'NONE', *, *, #7120, .F. ) ;
#4984 = ORIENTED_EDGE ( 'NONE', *, *, #7393, .T. ) ;
#4985 = VECTOR ( 'NONE', #15104, 1000.000000000000000 ) ;
#4986 = CARTESIAN_POINT ( 'NONE',  ( 0.000000000000000000, 23.00000000000000000, 0.000000000000000000 ) ) ;
#4987 = ORIENTED_EDGE ( 'NONE', *, *, #8897, .F. ) ;
#4988 = DIRECTION ( 'NONE',  ( -1.000000000000000000, 0.000000000000000000, 1.335138895993184054E-16 ) ) ;
#4989 = VECTOR ( 'NONE', #13376, 1000.000000000000000 ) ;
#4990 = AXIS2_PLACEMENT_3D ( 'NONE', #889, #16600, #5140 ) ;
#4991 = VERTEX_POINT ( 'NONE', #11821 ) ;
#4992 = EDGE_CURVE ( 'NONE', #7414, #14012, #6173, .T. ) ;
#4993 = EDGE_CURVE ( 'NONE', #5597, #9423, #3999, .T. ) ;
#4994 = VERTEX_POINT ( 'NONE', #15855 ) ;
#4995 = EDGE_CURVE ( 'NONE', #7039, #4299, #10031, .T. ) ;
#4996 = DIRECTION ( 'NONE',  ( 0.000000000000000000, 0.09950371902099770793, -0.9950371902099891530 ) ) ;
#4997 = DIRECTION ( 'NONE',  ( -0.000000000000000000, -1.000000000000000000, 0.000000000000000000 ) ) ;
#4998 = AXIS2_PLACEMENT_3D ( 'NONE', #11924, #2639, #10630 ) ;
#4999 = FACE_OUTER_BOUND ( 'NONE', #239, .T. ) ;
#5000 = CARTESIAN_POINT ( 'NONE',  ( -26.00000000000002842, 3.000000000000000000, 31.00000000000003908 ) ) ;
#5001 = DIRECTION ( 'NONE',  ( 1.000000000000000000, 0.000000000000000000, 0.000000000000000000 ) ) ;
#5002 = CARTESIAN_POINT ( 'NONE',  ( -40.00000000000000711, 10.00000000000000000, 26.00000000000000000 ) ) ;
#5003 = AXIS2_PLACEMENT_3D ( 'NONE', #7245, #13708, #12499 ) ;
#5004 = DIRECTION ( 'NONE',  ( 1.000000000000000000, 0.000000000000000000, 0.000000000000000000 ) ) ;
#5005 = AXIS2_PLACEMENT_3D ( 'NONE', #16144, #15963, #4209 ) ;
#5006 = ORIENTED_EDGE ( 'NONE', *, *, #15310, .F. ) ;
#5007 = DIRECTION ( 'NONE',  ( 0.000000000000000000, 0.000000000000000000, -1.000000000000000000 ) ) ;
#5008 = LINE ( 'NONE', #10174, #16808 ) ;
#5009 = ORIENTED_EDGE ( 'NONE', *, *, #7725, .T. ) ;
#5010 = CARTESIAN_POINT ( 'NONE',  ( 0.7366000000000316739, 217.7170024689957586, 287.2045212030222388 ) ) ;
#5012 = EDGE_LOOP ( 'NONE', ( #4397, #13768, #15049, #14951 ) ) ;
#5011 = ORIENTED_EDGE ( 'NONE', *, *, #12700, .T. ) ;
#5013 = CIRCLE ( 'NONE', #5275, 13.69540538389601991 ) ;
#5014 = ORIENTED_EDGE ( 'NONE', *, *, #10871, .F. ) ;
#5015 = AXIS2_PLACEMENT_3D ( 'NONE', #7577, #10346, #15576 ) ;
#5017 = CARTESIAN_POINT ( 'NONE',  ( 0.000000000000000000, 226.8713558223388134, -346.2582248962859808 ) ) ;
#5016 = CIRCLE ( 'NONE', #12176, 8.000000000000000000 ) ;
#5018 = CIRCLE ( 'NONE', #4735, 13.95000000000000107 ) ;
#5019 = CARTESIAN_POINT ( 'NONE',  ( 0.7366000000000039183, 192.7170024689955028, 37.20452120302225296 ) ) ;
#5020 = CARTESIAN_POINT ( 'NONE',  ( 37.50000000000000000, 196.3050121726289206, -75.00000000000000000 ) ) ;
#5021 = VERTEX_POINT ( 'NONE', #1347 ) ;
#5022 = CARTESIAN_POINT ( 'NONE',  ( -270.0000000000000000, 620.7506394335853201, -11.00000000000000000 ) ) ;
#5023 = ORIENTED_EDGE ( 'NONE', *, *, #16690, .F. ) ;
#5024 = CARTESIAN_POINT ( 'NONE',  ( 75.00000000000000000, 355.3192028797624857, -29.71049682360898814 ) ) ;
#5025 = FACE_OUTER_BOUND ( 'NONE', #11103, .T. ) ;
#5026 = FACE_OUTER_BOUND ( 'NONE', #5882, .T. ) ;
#5027 = AXIS2_PLACEMENT_3D ( 'NONE', #5862, #11019, #15130 ) ;
#5028 = AXIS2_PLACEMENT_3D ( 'NONE', #6276, #1061, #982 ) ;
#5029 = DIRECTION ( 'NONE',  ( 0.000000000000000000, 1.000000000000000000, 0.000000000000000000 ) ) ;
#5030 = VECTOR ( 'NONE', #1141, 1000.000000000000000 ) ;
#5031 = CARTESIAN_POINT ( 'NONE',  ( 2.204364238465236069E-16, 66.00000000000000000, -1.800000000000000711 ) ) ;
#5032 = EDGE_CURVE ( 'NONE', #7243, #12507, #2888, .T. ) ;
#5033 = VERTEX_POINT ( 'NONE', #7864 ) ;
#5034 = LINE ( 'NONE', #7607, #1234 ) ;
#5035 = EDGE_CURVE ( 'NONE', #1759, #1978, #6746, .T. ) ;
#5036 = CARTESIAN_POINT ( 'NONE',  ( -20.99999999999999645, 19.00000000000000000, 35.00000000000001421 ) ) ;
#5037 = DIRECTION ( 'NONE',  ( 0.000000000000000000, 0.000000000000000000, 1.000000000000000000 ) ) ;
#5038 = AXIS2_PLACEMENT_3D ( 'NONE', #15112, #14958, #7369 ) ;
#5039 = VERTEX_POINT ( 'NONE', #13121 ) ;
#5040 = AXIS2_PLACEMENT_3D ( 'NONE', #6868, #8350, #200 ) ;
#5041 = VECTOR ( 'NONE', #11433, 1000.000000000000000 ) ;
#5042 = DIRECTION ( 'NONE',  ( 0.000000000000000000, 0.000000000000000000, -1.000000000000000000 ) ) ;
#5043 = PRODUCT_DEFINITION ( 'UNKNOWN', '', #11940, #6352 ) ;
#5044 = CARTESIAN_POINT ( 'NONE',  ( 3.324999999999999734, 0.000000000000000000, 0.000000000000000000 ) ) ;
#5045 = VERTEX_POINT ( 'NONE', #14575 ) ;
#5046 = CARTESIAN_POINT ( 'NONE',  ( -210.0000000000000000, 512.1906115401388888, -11.00000000000000000 ) ) ;
#5047 = VECTOR ( 'NONE', #5138, 1000.000000000000000 ) ;
#5048 = CARTESIAN_POINT ( 'NONE',  ( -2.220446049250313081E-13, 135.5000000000000000, 3.000000000000000000 ) ) ;
#5049 = CARTESIAN_POINT ( 'NONE',  ( 39.09977993252476836, 344.7110430980827687, 0.000000000000000000 ) ) ;
#5050 = CARTESIAN_POINT ( 'NONE',  ( -55.99999999999989342, 549.5810598491746077, -513.4200196135282113 ) ) ;
#5051 = PRODUCT_DEFINITION_SHAPE ( 'NONE', 'NONE',  #13142 ) ;
#5052 = PLANE ( 'NONE',  #10979 ) ;
#5053 = CARTESIAN_POINT ( 'NONE',  ( -2.220446049250313081E-13, 75.00000000000001421, 0.000000000000000000 ) ) ;
#5054 = CARTESIAN_POINT ( 'NONE',  ( 55.99999999999989342, 523.2161522479888163, -489.1982331128240276 ) ) ;
#5055 = VERTEX_POINT ( 'NONE', #2893 ) ;
#5056 = EDGE_CURVE ( 'NONE', #9819, #5558, #3450, .T. ) ;
#5057 = DIRECTION ( 'NONE',  ( -0.000000000000000000, -1.000000000000000000, -0.000000000000000000 ) ) ;
#5058 = AXIS2_PLACEMENT_3D ( 'NONE', #14276, #5419, #14711 ) ;
#5059 = AXIS2_PLACEMENT_3D ( 'NONE', #4044, #7974, #13233 ) ;
#5060 = ITEM_DEFINED_TRANSFORMATION ( 'NONE', 'NONE', #672,  #1488 ) ;
#5061 = CIRCLE ( 'NONE', #8085, 17.85000000000000142 ) ;
#5062 = ORIENTED_EDGE ( 'NONE', *, *, #10871, .T. ) ;
#5063 = CARTESIAN_POINT ( 'NONE',  ( 22.99999999999999289, 68.00000000000000000, 37.00000000000002132 ) ) ;
#5064 = DIRECTION ( 'NONE',  ( -0.000000000000000000, -1.000000000000000000, -0.000000000000000000 ) ) ;
#5065 = ADVANCED_FACE ( 'NONE', ( #9514 ), #5547, .T. ) ;
#5066 = CARTESIAN_POINT ( 'NONE',  ( 1.250085104875786612E-12, 218.4499468633019603, 287.1312267635915987 ) ) ;
#5067 = ORIENTED_EDGE ( 'NONE', *, *, #16337, .F. ) ;
#5068 = PLANE ( 'NONE',  #15458 ) ;
#5069 = CARTESIAN_POINT ( 'NONE',  ( -46.99999999999988631, 523.2161522479893847, -585.8570079137933817 ) ) ;
#5070 = ORIENTED_EDGE ( 'NONE', *, *, #11399, .T. ) ;
#5071 = VECTOR ( 'NONE', #13554, 1000.000000000000000 ) ;
#5072 = DIRECTION ( 'NONE',  ( 0.000000000000000000, 1.000000000000000000, 0.000000000000000000 ) ) ;
#5073 = ORIENTED_EDGE ( 'NONE', *, *, #7824, .T. ) ;
#5074 = VERTEX_POINT ( 'NONE', #8133 ) ;
#5075 = EDGE_CURVE ( 'NONE', #10297, #11828, #4097, .T. ) ;
#5076 = DIRECTION ( 'NONE',  ( 0.000000000000000000, -0.9848077530122086864, 0.1736481776669273613 ) ) ;
#5077 = ORIENTED_EDGE ( 'NONE', *, *, #225, .T. ) ;
#5078 = DIRECTION ( 'NONE',  ( 0.000000000000000000, 0.000000000000000000, 1.000000000000000000 ) ) ;
#5079 = ORIENTED_EDGE ( 'NONE', *, *, #15759, .F. ) ;
#5080 = CIRCLE ( 'NONE', #9220, 9.000000000000007105 ) ;
#5081 = ORIENTED_EDGE ( 'NONE', *, *, #14921, .T. ) ;
#5082 = AXIS2_PLACEMENT_3D ( 'NONE', #12206, #5749, #9627 ) ;
#5083 = CARTESIAN_POINT ( 'NONE',  ( 26.00000000000000000, 19.00000000000000000, 31.00000000000003197 ) ) ;
#5084 = CARTESIAN_POINT ( 'NONE',  ( -2.220446049250313081E-13, 75.00000000000001421, 3.000000000000000000 ) ) ;
#5085 = EDGE_CURVE ( 'NONE', #1429, #295, #5283, .T. ) ;
#5086 = ORIENTED_EDGE ( 'NONE', *, *, #8643, .F. ) ;
#5087 = CARTESIAN_POINT ( 'NONE',  ( 0.000000000000000000, 50.00000000000000000, -36.50000000000000000 ) ) ;
#5088 = DIRECTION ( 'NONE',  ( -7.888609052210118054E-31, 0.000000000000000000, 1.000000000000000000 ) ) ;
#5089 = CARTESIAN_POINT ( 'NONE',  ( 45.00000000000000000, 473.6663340069158039, -561.9448123979092315 ) ) ;
#5090 = EDGE_CURVE ( 'NONE', #7931, #214, #14646, .T. ) ;
#5091 = EDGE_LOOP ( 'NONE', ( #13877, #4525, #2111, #1661, #1784, #7314 ) ) ;
#5092 = CARTESIAN_POINT ( 'NONE',  ( 394.0000000000001137, 240.0523724647196389, -17.15546574335979813 ) ) ;
#5093 = DIRECTION ( 'NONE',  ( 1.000000000000000000, -0.000000000000000000, 0.000000000000000000 ) ) ;
#5094 = ORIENTED_EDGE ( 'NONE', *, *, #9882, .T. ) ;
#5095 = EDGE_CURVE ( 'NONE', #16527, #2730, #2068, .T. ) ;
#5096 = VECTOR ( 'NONE', #8760, 1000.000000000000000 ) ;
#5097 = EDGE_CURVE ( 'NONE', #8336, #1044, #162, .T. ) ;
#5098 = CIRCLE ( 'NONE', #11979, 13.69540538389601991 ) ;
#5099 = EDGE_CURVE ( 'NONE', #10491, #3758, #13879, .T. ) ;
#5100 = DIRECTION ( 'NONE',  ( -1.000000000000000000, 0.000000000000000000, -0.000000000000000000 ) ) ;
#5101 = ORIENTED_EDGE ( 'NONE', *, *, #15624, .F. ) ;
#5102 = DIRECTION ( 'NONE',  ( 0.000000000000000000, 1.000000000000000000, 0.000000000000000000 ) ) ;
#5103 = ORIENTED_EDGE ( 'NONE', *, *, #3516, .F. ) ;
#5104 = ORIENTED_EDGE ( 'NONE', *, *, #14644, .T. ) ;
#5105 = DIRECTION ( 'NONE',  ( -0.000000000000000000, 1.000000000000000000, -0.000000000000000000 ) ) ;
#5106 = CARTESIAN_POINT ( 'NONE',  ( -31.00000000000003197, 0.000000000000000000, -22.99999999999999645 ) ) ;
#5107 = CARTESIAN_POINT ( 'NONE',  ( -20.99999999999999645, 8.000000000000000000, 35.00000000000001421 ) ) ;
#5108 = VECTOR ( 'NONE', #10368, 1000.000000000000000 ) ;
#5109 = ORIENTED_EDGE ( 'NONE', *, *, #829, .T. ) ;
#5110 = VECTOR ( 'NONE', #1835, 1000.000000000000000 ) ;
#5111 = DIRECTION ( 'NONE',  ( -1.000000000000000000, -0.000000000000000000, -0.000000000000000000 ) ) ;
#5112 = PLANE ( 'NONE',  #9714 ) ;
#5113 = DIRECTION ( 'NONE',  ( -0.000000000000000000, -0.000000000000000000, 1.000000000000000000 ) ) ;
#5114 = PLANE ( 'NONE',  #4565 ) ;
#5115 = CYLINDRICAL_SURFACE ( 'NONE', #11564, 3.000000000000002665 ) ;
#5116 = EDGE_CURVE ( 'NONE', #14016, #6668, #2105, .T. ) ;
#5117 = FACE_OUTER_BOUND ( 'NONE', #9622, .T. ) ;
#5118 = DIRECTION ( 'NONE',  ( -3.385371974912848683E-15, -0.9950371902099904853, 0.09950371902098585630 ) ) ;
#5120 = ORIENTED_EDGE ( 'NONE', *, *, #8266, .T. ) ;
#5119 = EDGE_LOOP ( 'NONE', ( #7382, #15872, #14797, #10354 ) ) ;
#5121 = VECTOR ( 'NONE', #5168, 1000.000000000000000 ) ;
#5122 = CARTESIAN_POINT ( 'NONE',  ( 34.00000000000002842, 3.000000000000000000, 23.00000000000000355 ) ) ;
#5123 = AXIS2_PLACEMENT_3D ( 'NONE', #10232, #10401, #3969 ) ;
#5124 = DIRECTION ( 'NONE',  ( 1.000000000000000000, -0.000000000000000000, 0.000000000000000000 ) ) ;
#5125 = LINE ( 'NONE', #7613, #84 ) ;
#5126 = EDGE_LOOP ( 'NONE', ( #14085, #8757, #4956, #6794 ) ) ;
#5127 = CYLINDRICAL_SURFACE ( 'NONE', #12687, 0.7366000000000004766 ) ;
#5128 = VECTOR ( 'NONE', #10558, 1000.000000000000000 ) ;
#5129 = FACE_OUTER_BOUND ( 'NONE', #4367, .T. ) ;
#5130 = VERTEX_POINT ( 'NONE', #12587 ) ;
#5131 = DIRECTION ( 'NONE',  ( 6.123031769111888756E-17, 0.000000000000000000, 1.000000000000000000 ) ) ;
#5132 = DIRECTION ( 'NONE',  ( -0.000000000000000000, -1.000000000000000000, -0.000000000000000000 ) ) ;
#5133 = DIRECTION ( 'NONE',  ( -1.000000000000000000, -0.000000000000000000, -0.000000000000000000 ) ) ;
#5134 = CARTESIAN_POINT ( 'NONE',  ( 415.3328573526671335, 308.8563596778320743, -10.00000000000000000 ) ) ;
#5135 = DIRECTION ( 'NONE',  ( 0.000000000000000000, 0.000000000000000000, -1.000000000000000000 ) ) ;
#5136 = DIRECTION ( 'NONE',  ( 1.000000000000000000, 0.000000000000000000, 0.000000000000000000 ) ) ;
#5137 = VERTEX_POINT ( 'NONE', #13641 ) ;
#5138 = DIRECTION ( 'NONE',  ( -0.000000000000000000, -1.000000000000000000, -0.000000000000000000 ) ) ;
#5139 = STYLED_ITEM ( 'NONE', ( #7101 ), #8514 ) ;
#5140 = DIRECTION ( 'NONE',  ( 0.000000000000000000, 0.000000000000000000, -1.000000000000000000 ) ) ;
#5141 = ORIENTED_EDGE ( 'NONE', *, *, #2768, .T. ) ;
#5142 = CARTESIAN_POINT ( 'NONE',  ( 394.0000000000001137, 240.7889724647196488, -17.15546574335979813 ) ) ;
#5143 = CARTESIAN_POINT ( 'NONE',  ( -22.00000000000001776, 8.000000000000000000, 33.00000000000000711 ) ) ;
#5144 = CARTESIAN_POINT ( 'NONE',  ( -5.000000000000000000, 0.000000000000000000, 18.46360580700775245 ) ) ;
#5145 = ORIENTED_EDGE ( 'NONE', *, *, #8083, .T. ) ;
#5146 = DIRECTION ( 'NONE',  ( 0.000000000000000000, 0.000000000000000000, 1.000000000000000000 ) ) ;
#5147 = CARTESIAN_POINT ( 'NONE',  ( 10.00000000000000000, 185.0000000000000000, -486.7326477857670852 ) ) ;
#5148 = ORIENTED_EDGE ( 'NONE', *, *, #16916, .F. ) ;
#5149 = AXIS2_PLACEMENT_3D ( 'NONE', #6197, #5959, #15147 ) ;
#5150 = CARTESIAN_POINT ( 'NONE',  ( 39.09977993252476836, 344.7110430980827687, -10.00000000000000000 ) ) ;
#5151 = EDGE_LOOP ( 'NONE', ( #32, #6064, #9289, #14099 ) ) ;
#5152 = VERTEX_POINT ( 'NONE', #9776 ) ;
#5153 = CARTESIAN_POINT ( 'NONE',  ( 394.0000000000001137, 339.1725919290084335, -110.6822657433597925 ) ) ;
#5154 = ORIENTED_EDGE ( 'NONE', *, *, #1317, .F. ) ;
#5155 = CARTESIAN_POINT ( 'NONE',  ( -2.255140518769849223E-14, 2.439454888092384977E-14, 8.368299999999997851 ) ) ;
#5156 = EDGE_CURVE ( 'NONE', #10758, #10732, #16290, .T. ) ;
#5157 = ORIENTED_EDGE ( 'NONE', *, *, #6981, .T. ) ;
#5158 = ORIENTED_EDGE ( 'NONE', *, *, #15505, .F. ) ;
#5159 = VECTOR ( 'NONE', #15539, 1000.000000000000227 ) ;
#5160 = DIRECTION ( 'NONE',  ( 0.000000000000000000, 0.000000000000000000, 1.000000000000000000 ) ) ;
#5161 = CARTESIAN_POINT ( 'NONE',  ( -55.99999999999989342, 493.2350855268086320, -508.1801094700848580 ) ) ;
#5162 = ADVANCED_FACE ( 'NONE', ( #12506 ), #7007, .T. ) ;
#5163 = ORIENTED_EDGE ( 'NONE', *, *, #8154, .F. ) ;
#5164 = LINE ( 'NONE', #10416, #14898 ) ;
#5165 = CARTESIAN_POINT ( 'NONE',  ( 22.99999999999998224, 10.00000000000000000, -36.99999999999999289 ) ) ;
#5166 = PLANE ( 'NONE',  #15183 ) ;
#5167 = ORIENTED_EDGE ( 'NONE', *, *, #7802, .F. ) ;
#5168 = DIRECTION ( 'NONE',  ( 0.000000000000000000, -1.000000000000000000, 0.000000000000000000 ) ) ;
#5169 = DIRECTION ( 'NONE',  ( 0.000000000000000000, 0.000000000000000000, 1.000000000000000000 ) ) ;
#5170 = ORIENTED_EDGE ( 'NONE', *, *, #13162, .T. ) ;
#5171 = DIRECTION ( 'NONE',  ( 0.000000000000000000, 0.000000000000000000, 1.000000000000000000 ) ) ;
#5172 = ORIENTED_EDGE ( 'NONE', *, *, #11498, .F. ) ;
#5173 = DIRECTION ( 'NONE',  ( -0.000000000000000000, -1.000000000000000000, -0.000000000000000000 ) ) ;
#5174 = EDGE_CURVE ( 'NONE', #15077, #10016, #15163, .T. ) ;
#5175 = ORIENTED_EDGE ( 'NONE', *, *, #4904, .T. ) ;
#5176 = CIRCLE ( 'NONE', #15349, 4.000000000000000000 ) ;
#5177 = ORIENTED_EDGE ( 'NONE', *, *, #4948, .T. ) ;
#5178 = PLANE ( 'NONE',  #7420 ) ;
#5179 = EDGE_CURVE ( 'NONE', #10304, #9656, #13794, .T. ) ;
#5180 = CARTESIAN_POINT ( 'NONE',  ( 17.99999999999998224, 6.000000000000000000, -35.99999999999999289 ) ) ;
#5182 = ORIENTED_EDGE ( 'NONE', *, *, #12426, .F. ) ;
#5181 = EDGE_CURVE ( 'NONE', #16882, #7581, #5973, .T. ) ;
#5184 = ADVANCED_FACE ( 'NONE', ( #8299 ), #11215, .T. ) ;
#5183 = DIRECTION ( 'NONE',  ( 0.000000000000000000, 0.000000000000000000, -1.000000000000000000 ) ) ;
#5185 = CARTESIAN_POINT ( 'NONE',  ( 64.99999999999998579, 380.0000000000000000, -17.00000000000000355 ) ) ;
#5186 = FACE_OUTER_BOUND ( 'NONE', #3654, .T. ) ;
#5187 = CARTESIAN_POINT ( 'NONE',  ( -31.00000000000005684, 10.00000000000000000, -23.00000000000000000 ) ) ;
#5188 = LINE ( 'NONE', #58, #5253 ) ;
#5189 = AXIS2_PLACEMENT_3D ( 'NONE', #3159, #13789, #12584 ) ;
#5190 = CYLINDRICAL_SURFACE ( 'NONE', #944, 22.50000000000000000 ) ;
#5191 = CARTESIAN_POINT ( 'NONE',  ( -31.81980515339462912, 11.00000000000000000, -28.51980515339464972 ) ) ;
#5193 = ORIENTED_EDGE ( 'NONE', *, *, #4267, .F. ) ;
#5192 = ORIENTED_EDGE ( 'NONE', *, *, #12849, .T. ) ;
#5194 = DIRECTION ( 'NONE',  ( -1.000000000000000000, 0.000000000000000000, 0.000000000000000000 ) ) ;
#5195 = VECTOR ( 'NONE', #10216, 1000.000000000000000 ) ;
#5196 = CARTESIAN_POINT ( 'NONE',  ( -55.99999999999989342, 549.5810598491746077, -518.1154249974242703 ) ) ;
#5197 = FACE_OUTER_BOUND ( 'NONE', #11968, .T. ) ;
#5198 = EDGE_CURVE ( 'NONE', #1964, #11502, #4363, .T. ) ;
#5199 = DIRECTION ( 'NONE',  ( 0.000000000000000000, 0.000000000000000000, -1.000000000000000000 ) ) ;
#5200 = EDGE_CURVE ( 'NONE', #1954, #9661, #9594, .T. ) ;
#5201 = AXIS2_PLACEMENT_3D ( 'NONE', #8852, #10455, #10626 ) ;
#5202 = ORIENTED_EDGE ( 'NONE', *, *, #6462, .T. ) ;
#5203 = VECTOR ( 'NONE', #1446, 1000.000000000000000 ) ;
#5204 = EDGE_CURVE ( 'NONE', #2454, #4908, #14918, .T. ) ;
#5205 = DIRECTION ( 'NONE',  ( 0.000000000000000000, 0.000000000000000000, 1.000000000000000000 ) ) ;
#5206 = CARTESIAN_POINT ( 'NONE',  ( 21.99999999999998224, 8.000000000000000000, -35.99999999999999289 ) ) ;
#5207 = ORIENTED_EDGE ( 'NONE', *, *, #8464, .T. ) ;
#5208 = DIRECTION ( 'NONE',  ( 1.000000000000000000, 0.000000000000000000, 0.000000000000000000 ) ) ;
#5209 = CARTESIAN_POINT ( 'NONE',  ( 437.7731165870194445, 329.6061121441327941, 0.000000000000000000 ) ) ;
#5210 = CARTESIAN_POINT ( 'NONE',  ( -35.00000000000000000, 19.00000000000000000, 20.99999999999999289 ) ) ;
#5211 = DIRECTION ( 'NONE',  ( -0.000000000000000000, -0.000000000000000000, 1.000000000000000000 ) ) ;
#5212 = CARTESIAN_POINT ( 'NONE',  ( 0.6999999999999999556, 0.000000000000000000, 0.000000000000000000 ) ) ;
#5213 = FACE_OUTER_BOUND ( 'NONE', #8952, .T. ) ;
#5214 = CARTESIAN_POINT ( 'NONE',  ( 9.454564816593551260E-13, 285.6351766110482231, 37.48264153682140432 ) ) ;
#5215 = ORIENTED_EDGE ( 'NONE', *, *, #11384, .T. ) ;
#5216 = CIRCLE ( 'NONE', #11813, 0.7366000000000039183 ) ;
#5217 = CARTESIAN_POINT ( 'NONE',  ( 39.09977993252476836, 344.7110430980827687, -6.736600000000000144 ) ) ;
#5218 = CONTEXT_DEPENDENT_SHAPE_REPRESENTATION ( #13694, #1924 ) ;
#5219 = DIRECTION ( 'NONE',  ( 1.000000000000000000, -0.000000000000000000, 3.854941057726254860E-16 ) ) ;
#5220 = ORIENTED_EDGE ( 'NONE', *, *, #7376, .T. ) ;
#5221 = DIRECTION ( 'NONE',  ( 0.000000000000000000, 0.000000000000000000, -1.000000000000000000 ) ) ;
#5222 = DIRECTION ( 'NONE',  ( 1.000000000000000000, 0.000000000000000000, -0.000000000000000000 ) ) ;
#5223 = AXIS2_PLACEMENT_3D ( 'NONE', #5263, #6466, #9242 ) ;
#5224 = DIRECTION ( 'NONE',  ( 0.000000000000000000, 0.000000000000000000, 1.000000000000000000 ) ) ;
#5225 = ORIENTED_EDGE ( 'NONE', *, *, #695, .T. ) ;
#5226 = DIRECTION ( 'NONE',  ( -1.000000000000000000, -0.000000000000000000, -0.000000000000000000 ) ) ;
#5227 = DIRECTION ( 'NONE',  ( -0.000000000000000000, -1.000000000000000000, -0.000000000000000000 ) ) ;
#5228 = FACE_OUTER_BOUND ( 'NONE', #12131, .T. ) ;
#5229 = VERTEX_POINT ( 'NONE', #3162 ) ;
#5230 = CYLINDRICAL_SURFACE ( 'NONE', #13824, 2.500000000000002220 ) ;
#5231 = ORIENTED_EDGE ( 'NONE', *, *, #498, .F. ) ;
#5232 = EDGE_LOOP ( 'NONE', ( #6099, #4087, #13429, #8171, #16045 ) ) ;
#5233 = CARTESIAN_POINT ( 'NONE',  ( 0.000000000000000000, 240.0523724647196389, -110.6822657433598067 ) ) ;
#5234 = ORIENTED_EDGE ( 'NONE', *, *, #5, .T. ) ;
#5235 = EDGE_CURVE ( 'NONE', #9318, #414, #578, .T. ) ;
#5236 = DIRECTION ( 'NONE',  ( 0.000000000000000000, 0.000000000000000000, 1.000000000000000000 ) ) ;
#5237 = AXIS2_PLACEMENT_3D ( 'NONE', #10845, #14534, #370 ) ;
#5238 = VERTEX_POINT ( 'NONE', #8476 ) ;
#5239 = ORIENTED_EDGE ( 'NONE', *, *, #2873, .T. ) ;
#5240 = CIRCLE ( 'NONE', #14869, 12.50000000000001066 ) ;
#5241 = LINE ( 'NONE', #8962, #6900 ) ;
#5242 = LINE ( 'NONE', #15899, #16563 ) ;
#5243 = ORIENTED_EDGE ( 'NONE', *, *, #22, .F. ) ;
#5244 = FACE_OUTER_BOUND ( 'NONE', #4900, .T. ) ;
#5245 = CARTESIAN_POINT ( 'NONE',  ( 1.286622718088548112E-12, 260.4765148507136701, 287.1312267635912008 ) ) ;
#5246 = AXIS2_PLACEMENT_3D ( 'NONE', #4463, #3435, #12532 ) ;
#5247 = EDGE_CURVE ( 'NONE', #5278, #11935, #1938, .T. ) ;
#5248 = DIRECTION ( 'NONE',  ( -0.9998870921963913805, -0.01502673813723916230, -0.000000000000000000 ) ) ;
#5249 = ORIENTED_EDGE ( 'NONE', *, *, #663, .F. ) ;
#5250 = DIRECTION ( 'NONE',  ( -0.000000000000000000, 1.000000000000000000, -0.000000000000000000 ) ) ;
#5251 = CARTESIAN_POINT ( 'NONE',  ( 55.99999999999989342, 473.6663340069157471, -545.1966447803968094 ) ) ;
#5252 = EDGE_LOOP ( 'NONE', ( #6435, #7413, #11771, #323 ) ) ;
#5253 = VECTOR ( 'NONE', #10529, 1000.000000000000000 ) ;
#5254 = VECTOR ( 'NONE', #3225, 1000.000000000000000 ) ;
#5255 = CARTESIAN_POINT ( 'NONE',  ( -37.00000000000000000, 0.000000000000000000, -22.99999999999999645 ) ) ;
#5256 = ORIENTED_EDGE ( 'NONE', *, *, #189, .F. ) ;
#5257 = EDGE_CURVE ( 'NONE', #386, #1641, #15237, .T. ) ;
#5258 = DIRECTION ( 'NONE',  ( -0.000000000000000000, -1.000000000000000000, -0.000000000000000000 ) ) ;
#5259 = EDGE_LOOP ( 'NONE', ( #12042, #6069, #9784, #3513 ) ) ;
#5260 = AXIS2_PLACEMENT_3D ( 'NONE', #3686, #16890, #15612 ) ;
#5261 = VERTEX_POINT ( 'NONE', #8731 ) ;
#5262 = CARTESIAN_POINT ( 'NONE',  ( 21.00000000000000000, 19.00000000000000000, -31.00000000000003908 ) ) ;
#5263 = CARTESIAN_POINT ( 'NONE',  ( 30.99999999999997868, 10.00000000000000000, -30.99999999999999645 ) ) ;
#5264 = DIRECTION ( 'NONE',  ( 0.000000000000000000, 0.000000000000000000, -1.000000000000000000 ) ) ;
#5265 = VERTEX_POINT ( 'NONE', #996 ) ;
#5266 = VECTOR ( 'NONE', #2996, 1000.000000000000000 ) ;
#5267 = DIRECTION ( 'NONE',  ( 1.000000000000000000, 0.000000000000000000, 1.156482317317870344E-15 ) ) ;
#5268 = VECTOR ( 'NONE', #12444, 1000.000000000000000 ) ;
#5269 = DIRECTION ( 'NONE',  ( 1.000000000000000000, -0.000000000000000000, 3.854941057726249930E-16 ) ) ;
#5270 = ADVANCED_FACE ( 'NONE', ( #8980, #10353 ), #14293, .T. ) ;
#5271 = CYLINDRICAL_SURFACE ( 'NONE', #14557, 2.500000000000002220 ) ;
#5272 = EDGE_CURVE ( 'NONE', #7648, #2603, #15511, .T. ) ;
#5273 = CARTESIAN_POINT ( 'NONE',  ( 0.000000000000000000, 364.9870314427736275, -216.3519347178565795 ) ) ;
#5274 = DIRECTION ( 'NONE',  ( 0.01502673813723916403, -0.9998870921963913805, 0.000000000000000000 ) ) ;
#5275 = AXIS2_PLACEMENT_3D ( 'NONE', #15826, #1312, #6360 ) ;
#5276 = DIRECTION ( 'NONE',  ( -0.000000000000000000, 0.000000000000000000, -1.000000000000000000 ) ) ;
#5277 = DIRECTION ( 'NONE',  ( 1.000000000000000000, -0.000000000000000000, -0.000000000000000000 ) ) ;
#5279 = EDGE_LOOP ( 'NONE', ( #9386, #4057, #8181, #3599 ) ) ;
#5278 = VERTEX_POINT ( 'NONE', #12917 ) ;
#5280 = EDGE_CURVE ( 'NONE', #10097, #13856, #15335, .T. ) ;
#5281 = VECTOR ( 'NONE', #2952, 1000.000000000000000 ) ;
#5282 = ADVANCED_FACE ( 'NONE', ( #16530 ), #14693, .T. ) ;
#5283 = LINE ( 'NONE', #9337, #4539 ) ;
#5284 = EDGE_CURVE ( 'NONE', #6577, #1719, #2356, .T. ) ;
#5285 = ADVANCED_FACE ( 'NONE', ( #1072 ), #2522, .F. ) ;
#5286 = AXIS2_PLACEMENT_3D ( 'NONE', #13008, #1320, #4847 ) ;
#5287 = AXIS2_PLACEMENT_3D ( 'NONE', #3323, #15339, #8402 ) ;
#5288 = CARTESIAN_POINT ( 'NONE',  ( 0.01917172636707389216, 285.6351388618906526, 37.48263776190567853 ) ) ;
#5289 = CARTESIAN_POINT ( 'NONE',  ( -31.00000000000002132, 10.00000000000000000, -31.00000000000000000 ) ) ;
#5290 = CARTESIAN_POINT ( 'NONE',  ( 0.7365999999999761627, 286.2094592450219466, 37.20452120302238086 ) ) ;
#5291 = VECTOR ( 'NONE', #3390, 1000.000000000000000 ) ;
#5292 = EDGE_LOOP ( 'NONE', ( #13203, #12313, #3125, #916 ) ) ;
#5293 = CARTESIAN_POINT ( 'NONE',  ( 2.999999999999996891, 60.00000000000000711, 6.000000000000000000 ) ) ;
#5294 = CIRCLE ( 'NONE', #7222, 9.000000000000007105 ) ;
#5295 = AXIS2_PLACEMENT_3D ( 'NONE', #7673, #12927, #313 ) ;
#5296 = FACE_OUTER_BOUND ( 'NONE', #3877, .T. ) ;
#5298 = EDGE_CURVE ( 'NONE', #14722, #15314, #12240, .T. ) ;
#5297 = EDGE_LOOP ( 'NONE', ( #6039, #9641, #16859, #7301 ) ) ;
#5299 = PLANE ( 'NONE',  #841 ) ;
#5300 = VECTOR ( 'NONE', #12825, 1000.000000000000000 ) ;
#5301 = DIRECTION ( 'NONE',  ( -0.000000000000000000, -1.000000000000000000, -0.000000000000000000 ) ) ;
#5302 = ORIENTED_EDGE ( 'NONE', *, *, #9729, .T. ) ;
#5303 = AXIS2_PLACEMENT_3D ( 'NONE', #493, #410, #16114 ) ;
#5304 = LINE ( 'NONE', #15787, #15136 ) ;
#5305 = FACE_OUTER_BOUND ( 'NONE', #16675, .T. ) ;
#5306 = CARTESIAN_POINT ( 'NONE',  ( 1.286622718088565479E-12, 285.4366476906530465, 37.52989836422118941 ) ) ;
#5307 = ORIENTED_EDGE ( 'NONE', *, *, #6648, .F. ) ;
#5308 = EDGE_CURVE ( 'NONE', #10947, #9234, #16866, .T. ) ;
#5309 = AXIS2_PLACEMENT_3D ( 'NONE', #2157, #10150, #4641 ) ;
#5310 = ADVANCED_FACE ( 'NONE', ( #8809 ), #9494, .T. ) ;
#5311 = EDGE_CURVE ( 'NONE', #352, #14044, #12759, .T. ) ;
#5312 = LINE ( 'NONE', #7968, #3704 ) ;
#5313 = ADVANCED_FACE ( 'NONE', ( #15254 ), #7415, .F. ) ;
#5314 = CIRCLE ( 'NONE', #12464, 4.999999999999997335 ) ;
#5315 =( GEOMETRIC_REPRESENTATION_CONTEXT ( 3 ) GLOBAL_UNCERTAINTY_ASSIGNED_CONTEXT ( ( #2925 ) ) GLOBAL_UNIT_ASSIGNED_CONTEXT ( ( #7545, #2655, #7887 ) ) REPRESENTATION_CONTEXT ( 'NONE', 'WORKASPACE' ) );
#5316 = CIRCLE ( 'NONE', #7503, 0.9999999999999950040 ) ;
#5317 = CARTESIAN_POINT ( 'NONE',  ( 34.99999999999997868, 11.00000000000000000, 40.00000000000000711 ) ) ;
#5318 = ORIENTED_EDGE ( 'NONE', *, *, #10215, .T. ) ;
#5319 = AXIS2_PLACEMENT_3D ( 'NONE', #8870, #11775, #11862 ) ;
#5320 = DIRECTION ( 'NONE',  ( 6.092845550116204443E-17, 0.09950371902098714694, 0.9950371902099903743 ) ) ;
#5321 = UNCERTAINTY_MEASURE_WITH_UNIT (LENGTH_MEASURE( 1.000000000000000082E-05 ), #15914, 'distance_accuracy_value', 'NONE');
#5322 = FACE_OUTER_BOUND ( 'NONE', #41, .T. ) ;
#5323 = LINE ( 'NONE', #3790, #8789 ) ;
#5324 = ORIENTED_EDGE ( 'NONE', *, *, #566, .T. ) ;
#5325 = LINE ( 'NONE', #4047, #3669 ) ;
#5326 = LINE ( 'NONE', #15810, #7615 ) ;
#5327 = CARTESIAN_POINT ( 'NONE',  ( 31.00000000000000000, 8.000000000000000000, -21.00000000000000355 ) ) ;
#5328 = ORIENTED_EDGE ( 'NONE', *, *, #2646, .T. ) ;
#5329 = AXIS2_PLACEMENT_3D ( 'NONE', #10566, #5222, #10477 ) ;
#5330 = EDGE_LOOP ( 'NONE', ( #13524, #14981, #12400, #626 ) ) ;
#5331 = APPLICATION_CONTEXT ( 'automotive_design' ) ;
#5332 = ORIENTED_EDGE ( 'NONE', *, *, #8121, .T. ) ;
#5333 = LINE ( 'NONE', #6959, #1494 ) ;
#5334 = AXIS2_PLACEMENT_3D ( 'NONE', #2042, #3085, #8417 ) ;
#5335 = EDGE_CURVE ( 'NONE', #3462, #12242, #11633, .T. ) ;
#5336 = VERTEX_POINT ( 'NONE', #3657 ) ;
#5337 = ORIENTED_EDGE ( 'NONE', *, *, #15357, .T. ) ;
#5338 = CARTESIAN_POINT ( 'NONE',  ( 139.9999999999999716, -5.551115123125782702E-14, 10.35193471785655817 ) ) ;
#5339 = ORIENTED_EDGE ( 'NONE', *, *, #2398, .T. ) ;
#5340 = ORIENTED_EDGE ( 'NONE', *, *, #8399, .F. ) ;
#5341 = PRODUCT_DEFINITION_FORMATION_WITH_SPECIFIED_SOURCE ( 'ANY', '', #12073, .NOT_KNOWN. ) ;
#5342 = DIRECTION ( 'NONE',  ( -1.000000000000000000, 0.000000000000000000, 0.000000000000000000 ) ) ;
#5343 = DIRECTION ( 'NONE',  ( -0.000000000000000000, 1.000000000000000000, -0.000000000000000000 ) ) ;
#5344 = ORIENTED_EDGE ( 'NONE', *, *, #14773, .F. ) ;
#5345 = CIRCLE ( 'NONE', #9469, 5.000000000000000888 ) ;
#5346 = CARTESIAN_POINT ( 'NONE',  ( -55.99999999999989342, 523.2161522479888163, -516.5890438806160319 ) ) ;
#5347 = ADVANCED_FACE ( 'NONE', ( #8902 ), #3818, .T. ) ;
#5348 = FACE_BOUND ( 'NONE', #11004, .T. ) ;
#5349 = VERTEX_POINT ( 'NONE', #10273 ) ;
#5350 = VERTEX_POINT ( 'NONE', #15510 ) ;
#5351 = FACE_OUTER_BOUND ( 'NONE', #1207, .T. ) ;
#5352 = DIRECTION ( 'NONE',  ( 0.000000000000000000, 1.000000000000000000, 0.000000000000000000 ) ) ;
#5353 = ORIENTED_EDGE ( 'NONE', *, *, #7819, .T. ) ;
#5354 = EDGE_CURVE ( 'NONE', #14978, #352, #7663, .T. ) ;
#5355 = CYLINDRICAL_SURFACE ( 'NONE', #13736, 0.9999999999999965583 ) ;
#5356 = EDGE_LOOP ( 'NONE', ( #12269, #3020, #13352, #14960, #11921, #10629 ) ) ;
#5357 = FACE_OUTER_BOUND ( 'NONE', #6218, .T. ) ;
#5358 = CIRCLE ( 'NONE', #12488, 4.999999999999997335 ) ;
#5359 = EDGE_LOOP ( 'NONE', ( #3465, #13829, #203, #10926 ) ) ;
#5360 = EDGE_LOOP ( 'NONE', ( #6869, #635, #12486, #16034 ) ) ;
#5361 = FACE_OUTER_BOUND ( 'NONE', #1262, .T. ) ;
#5362 = CARTESIAN_POINT ( 'NONE',  ( -46.99999999999988631, 473.6663340069157471, -531.5012393965008641 ) ) ;
#5363 = DIRECTION ( 'NONE',  ( 1.000000000000000000, 0.000000000000000000, 0.000000000000000000 ) ) ;
#5364 = EDGE_LOOP ( 'NONE', ( #3438, #7822 ) ) ;
#5365 = DIRECTION ( 'NONE',  ( -1.000000000000000000, 0.000000000000000000, 0.000000000000000000 ) ) ;
#5366 = LINE ( 'NONE', #5712, #15462 ) ;
#5367 = AXIS2_PLACEMENT_3D ( 'NONE', #2643, #11575, #6322 ) ;
#5368 = LINE ( 'NONE', #14745, #1933 ) ;
#5369 = CIRCLE ( 'NONE', #10863, 5.000000000000000888 ) ;
#5370 = CARTESIAN_POINT ( 'NONE',  ( 6.649999999999999467, 18.17500000000000071, 0.000000000000000000 ) ) ;
#5371 = CARTESIAN_POINT ( 'NONE',  ( 25.99999999999997868, 0.000000000000000000, 40.00000000000000711 ) ) ;
#5372 = CARTESIAN_POINT ( 'NONE',  ( 2.999999999999996891, 60.00000000000000711, 6.000000000000000000 ) ) ;
#5373 = DIRECTION ( 'NONE',  ( 1.000000000000000000, -0.000000000000000000, 0.000000000000000000 ) ) ;
#5375 = ORIENTED_EDGE ( 'NONE', *, *, #14643, .F. ) ;
#5374 = ORIENTED_EDGE ( 'NONE', *, *, #4689, .F. ) ;
#5376 = DIRECTION ( 'NONE',  ( 0.000000000000000000, 1.000000000000000000, 0.000000000000000000 ) ) ;
#5377 = CIRCLE ( 'NONE', #12796, 13.69540538389601991 ) ;
#5378 = CARTESIAN_POINT ( 'NONE',  ( -1.725642888253169360, 288.6479481343113775, 37.61614439054952896 ) ) ;
#5379 = EDGE_CURVE ( 'NONE', #16667, #6128, #3459, .T. ) ;
#5380 = AXIS2_PLACEMENT_3D ( 'NONE', #3773, #3851, #7874 ) ;
#5381 = DIRECTION ( 'NONE',  ( 0.000000000000000000, 1.000000000000000000, 1.224646799147353207E-16 ) ) ;
#5382 = PLANE ( 'NONE',  #13542 ) ;
#5383 = ORIENTED_EDGE ( 'NONE', *, *, #6662, .F. ) ;
#5384 = PLANE ( 'NONE',  #3107 ) ;
#5385 = EDGE_CURVE ( 'NONE', #5942, #10179, #9493, .T. ) ;
#5386 = FACE_OUTER_BOUND ( 'NONE', #4580, .T. ) ;
#5387 = ORIENTED_EDGE ( 'NONE', *, *, #14777, .T. ) ;
#5388 = DIRECTION ( 'NONE',  ( 0.000000000000000000, 1.000000000000000000, 0.000000000000000000 ) ) ;
#5389 = DIRECTION ( 'NONE',  ( -1.000000000000000000, -0.000000000000000000, -0.000000000000000000 ) ) ;
#5390 = DIRECTION ( 'NONE',  ( 0.000000000000000000, 0.000000000000000000, 1.000000000000000000 ) ) ;
#5391 = CIRCLE ( 'NONE', #16647, 4.695405383896011919 ) ;
#5392 = VECTOR ( 'NONE', #3210, 1000.000000000000000 ) ;
#5393 = DIRECTION ( 'NONE',  ( 0.000000000000000000, 1.000000000000000000, 0.000000000000000000 ) ) ;
#5394 = LINE ( 'NONE', #6681, #8828 ) ;
#5395 = ORIENTED_EDGE ( 'NONE', *, *, #12644, .F. ) ;
#5396 = DIRECTION ( 'NONE',  ( 0.000000000000000000, 1.000000000000000000, 0.000000000000000000 ) ) ;
#5397 = FACE_OUTER_BOUND ( 'NONE', #10882, .T. ) ;
#5398 = EDGE_CURVE ( 'NONE', #1379, #8348, #5369, .T. ) ;
#5399 = LINE ( 'NONE', #11679, #886 ) ;
#5400 = VECTOR ( 'NONE', #784, 1000.000000000000000 ) ;
#5401 = ORIENTED_EDGE ( 'NONE', *, *, #14986, .F. ) ;
#5402 = FACE_OUTER_BOUND ( 'NONE', #830, .T. ) ;
#5403 = EDGE_CURVE ( 'NONE', #12347, #16344, #14704, .T. ) ;
#5404 = DIRECTION ( 'NONE',  ( -1.000000000000000000, 0.000000000000000000, 6.123233995736766036E-17 ) ) ;
#5405 = ADVANCED_FACE ( 'NONE', ( #14385 ), #2870, .F. ) ;
#5406 = EDGE_CURVE ( 'NONE', #6577, #11977, #15916, .T. ) ;
#5407 = DIRECTION ( 'NONE',  ( 0.000000000000000000, 1.000000000000000000, 0.000000000000000000 ) ) ;
#5408 = EDGE_LOOP ( 'NONE', ( #10024, #15896, #13748, #5077, #10210, #6021, #10564, #12791, #9643, #1885, #4851, #257, #12671, #16494, #16816, #16693 ) ) ;
#5409 = DIRECTION ( 'NONE',  ( 0.000000000000000000, 0.000000000000000000, 1.000000000000000000 ) ) ;
#5410 = EDGE_CURVE ( 'NONE', #15604, #7379, #2698, .T. ) ;
#5411 = CARTESIAN_POINT ( 'NONE',  ( -18.00000000000001421, 10.00000000000000000, 36.00000000000000711 ) ) ;
#5412 = CARTESIAN_POINT ( 'NONE',  ( 394.0000000000001137, 451.4647406485094621, 28.44173619839933309 ) ) ;
#5413 = ORIENTED_EDGE ( 'NONE', *, *, #6337, .F. ) ;
#5414 = SURFACE_STYLE_USAGE ( .BOTH. , #195 ) ;
#5415 = ORIENTED_EDGE ( 'NONE', *, *, #9078, .T. ) ;
#5416 = ORIENTED_EDGE ( 'NONE', *, *, #8895, .F. ) ;
#5417 = CARTESIAN_POINT ( 'NONE',  ( 18.99999999999998224, 8.000000000000000000, -39.99999999999999289 ) ) ;
#5418 = ORIENTED_EDGE ( 'NONE', *, *, #3834, .T. ) ;
#5419 = DIRECTION ( 'NONE',  ( 0.000000000000000000, 0.000000000000000000, 1.000000000000000000 ) ) ;
#5420 = ORIENTED_EDGE ( 'NONE', *, *, #879, .T. ) ;
#5421 = VERTEX_POINT ( 'NONE', #4159 ) ;
#5422 = CARTESIAN_POINT ( 'NONE',  ( -22.00000000000001776, 6.000000000000000000, 36.00000000000000711 ) ) ;
#5423 = EDGE_CURVE ( 'NONE', #13185, #4106, #7928, .T. ) ;
#5424 = DIRECTION ( 'NONE',  ( -1.000000000000000000, 0.000000000000000000, 0.000000000000000000 ) ) ;
#5425 = VERTEX_POINT ( 'NONE', #14734 ) ;
#5426 = DIRECTION ( 'NONE',  ( 1.000000000000000000, 0.000000000000000000, 0.000000000000000000 ) ) ;
#5427 = ADVANCED_FACE ( 'NONE', ( #2616 ), #304, .F. ) ;
#5428 = AXIS2_PLACEMENT_3D ( 'NONE', #12492, #12827, #1059 ) ;
#5429 = FACE_OUTER_BOUND ( 'NONE', #16389, .T. ) ;
#5430 = EDGE_LOOP ( 'NONE', ( #4117, #16806, #781, #11046 ) ) ;
#5431 = DIRECTION ( 'NONE',  ( 0.000000000000000000, 1.000000000000000000, 0.000000000000000000 ) ) ;
#5432 = ORIENTED_EDGE ( 'NONE', *, *, #11496, .F. ) ;
#5433 = LINE ( 'NONE', #14726, #12284 ) ;
#5434 = DIRECTION ( 'NONE',  ( -1.000000000000000000, 0.000000000000000000, 0.000000000000000000 ) ) ;
#5435 = EDGE_LOOP ( 'NONE', ( #9938, #10852, #14677, #1768, #6280, #15825, #634, #12462, #931, #6446, #7362, #11820, #14365, #4815, #5951, #16883 ) ) ;
#5436 = CARTESIAN_POINT ( 'NONE',  ( 0.000000000000000000, 380.0000000000000000, 0.000000000000000000 ) ) ;
#5437 = ORIENTED_EDGE ( 'NONE', *, *, #10531, .T. ) ;
#5438 = DIRECTION ( 'NONE',  ( -0.6031630618355670048, -1.916859900632332136E-19, 0.7976179040349731242 ) ) ;
#5439 = CARTESIAN_POINT ( 'NONE',  ( 31.00000000000000711, 68.00000000000000000, -30.99999999999999289 ) ) ;
#5440 = CIRCLE ( 'NONE', #6253, 2.500000000000002220 ) ;
#5441 = ORIENTED_EDGE ( 'NONE', *, *, #2986, .T. ) ;
#5442 = EDGE_CURVE ( 'NONE', #10865, #10595, #5523, .T. ) ;
#5443 = ORIENTED_EDGE ( 'NONE', *, *, #8154, .T. ) ;
#5444 =( NAMED_UNIT ( * ) PLANE_ANGLE_UNIT ( ) SI_UNIT ( $, .RADIAN. ) );
#5445 = CARTESIAN_POINT ( 'NONE',  ( 3.324999999999999734, -12.97499999999999964, -1.588979221893690953E-15 ) ) ;
#5446 = PLANE ( 'NONE',  #7484 ) ;
#5447 = ORIENTED_EDGE ( 'NONE', *, *, #2385, .T. ) ;
#5448 = DIRECTION ( 'NONE',  ( 0.000000000000000000, 0.000000000000000000, -1.000000000000000000 ) ) ;
#5449 = DIRECTION ( 'NONE',  ( 0.000000000000000000, 0.000000000000000000, 1.000000000000000000 ) ) ;
#5450 = DIRECTION ( 'NONE',  ( 0.000000000000000000, 1.000000000000000000, 0.000000000000000000 ) ) ;
#5451 = DIRECTION ( 'NONE',  ( 1.000000000000000000, 0.000000000000000000, -0.000000000000000000 ) ) ;
#5452 = CARTESIAN_POINT ( 'NONE',  ( 39.99999999999999289, 0.000000000000000000, 26.00000000000000000 ) ) ;
#5453 = VECTOR ( 'NONE', #2374, 1000.000000000000000 ) ;
#5454 = PLANE ( 'NONE',  #7227 ) ;
#5455 = LINE ( 'NONE', #8208, #10154 ) ;
#5457 = VERTEX_POINT ( 'NONE', #14555 ) ;
#5456 = ORIENTED_EDGE ( 'NONE', *, *, #6557, .F. ) ;
#5458 = CARTESIAN_POINT ( 'NONE',  ( -23.00000000000002132, 10.00000000000000000, 32.00000000000000711 ) ) ;
#5459 = CARTESIAN_POINT ( 'NONE',  ( -2.792885358480770019, 287.4741092055357399, 37.59942507683089019 ) ) ;
#5460 = DIRECTION ( 'NONE',  ( 0.000000000000000000, 0.000000000000000000, 1.000000000000000000 ) ) ;
#5461 = DIRECTION ( 'NONE',  ( 0.000000000000000000, 0.000000000000000000, -1.000000000000000000 ) ) ;
#5462 = EDGE_LOOP ( 'NONE', ( #3826, #938, #4927, #13393 ) ) ;
#5463 = CARTESIAN_POINT ( 'NONE',  ( 46.99999999999988631, 523.2161522479893847, -585.8570079137933817 ) ) ;
#5464 = VECTOR ( 'NONE', #3117, 1000.000000000000000 ) ;
#5465 = DIRECTION ( 'NONE',  ( 0.000000000000000000, 0.000000000000000000, 1.000000000000000000 ) ) ;
#5466 = ORIENTED_EDGE ( 'NONE', *, *, #12740, .T. ) ;
#5467 = DIRECTION ( 'NONE',  ( 1.000000000000000000, -0.000000000000000000, -0.000000000000000000 ) ) ;
#5468 = DIRECTION ( 'NONE',  ( -0.000000000000000000, 0.000000000000000000, 1.000000000000000000 ) ) ;
#5469 = LINE ( 'NONE', #4375, #10193 ) ;
#5470 = EDGE_CURVE ( 'NONE', #11540, #14941, #11983, .T. ) ;
#5471 = LINE ( 'NONE', #2913, #12943 ) ;
#5472 =( NAMED_UNIT ( * ) SI_UNIT ( $, .STERADIAN. ) SOLID_ANGLE_UNIT ( ) );
#5473 = DIRECTION ( 'NONE',  ( 0.000000000000000000, -9.899245676326632924E-17, -1.000000000000000000 ) ) ;
#5474 = ORIENTED_EDGE ( 'NONE', *, *, #3121, .T. ) ;
#5475 = CARTESIAN_POINT ( 'NONE',  ( 0.000000000000000000, 0.000000000000000000, 0.000000000000000000 ) ) ;
#5476 = EDGE_CURVE ( 'NONE', #7039, #16578, #8405, .T. ) ;
#5477 = VECTOR ( 'NONE', #10014, 1000.000000000000000 ) ;
#5478 = DIRECTION ( 'NONE',  ( -0.000000000000000000, -1.000000000000000000, -0.000000000000000000 ) ) ;
#5479 = VECTOR ( 'NONE', #3078, 999.9999999999998863 ) ;
#5480 = EDGE_LOOP ( 'NONE', ( #106, #1025, #14897, #633 ) ) ;
#5481 = DIRECTION ( 'NONE',  ( 0.000000000000000000, 0.000000000000000000, -1.000000000000000000 ) ) ;
#5482 = UNCERTAINTY_MEASURE_WITH_UNIT (LENGTH_MEASURE( 1.000000000000000082E-05 ), #4737, 'distance_accuracy_value', 'NONE');
#5483 = DIRECTION ( 'NONE',  ( 0.000000000000000000, 1.000000000000000000, 0.000000000000000000 ) ) ;
#5484 = CARTESIAN_POINT ( 'NONE',  ( 55.99999999999989342, 523.2161522479888163, -498.1982331128240276 ) ) ;
#5485 = ORIENTED_EDGE ( 'NONE', *, *, #9975, .T. ) ;
#5486 = CARTESIAN_POINT ( 'NONE',  ( 1.250085104875786612E-12, 220.0768326692952996, 286.9685381829922903 ) ) ;
#5487 = LINE ( 'NONE', #10734, #3514 ) ;
#5488 = CARTESIAN_POINT ( 'NONE',  ( 394.0000000000001137, 240.7889724647196488, -16.41886574335980242 ) ) ;
#5489 = VERTEX_POINT ( 'NONE', #16008 ) ;
#5490 = CIRCLE ( 'NONE', #12625, 7.500000000000003553 ) ;
#5491 = ADVANCED_FACE ( 'NONE', ( #6461 ), #16943, .F. ) ;
#5492 =( NAMED_UNIT ( * ) PLANE_ANGLE_UNIT ( ) SI_UNIT ( $, .RADIAN. ) );
#5493 = ADVANCED_FACE ( 'NONE', ( #10603, #5357 ), #6544, .T. ) ;
#5494 = EDGE_LOOP ( 'NONE', ( #13010, #142, #15634, #14020 ) ) ;
#5495 = ORIENTED_EDGE ( 'NONE', *, *, #11827, .T. ) ;
#5496 = FACE_OUTER_BOUND ( 'NONE', #15207, .T. ) ;
#5497 = STYLED_ITEM ( 'NONE', ( #6245 ), #3244 ) ;
#5498 = ORIENTED_EDGE ( 'NONE', *, *, #8340, .F. ) ;
#5499 = EDGE_CURVE ( 'NONE', #9832, #14585, #15750, .T. ) ;
#5500 = DIRECTION ( 'NONE',  ( 0.000000000000000000, 0.000000000000000000, 1.000000000000000000 ) ) ;
#5501 = EDGE_CURVE ( 'NONE', #7500, #4414, #5647, .T. ) ;
#5502 = EDGE_CURVE ( 'NONE', #6345, #8690, #8014, .T. ) ;
#5503 = ORIENTED_EDGE ( 'NONE', *, *, #9846, .T. ) ;
#5504 = AXIS2_PLACEMENT_3D ( 'NONE', #6485, #11744, #13027 ) ;
#5505 = ORIENTED_EDGE ( 'NONE', *, *, #4402, .T. ) ;
#5506 = CARTESIAN_POINT ( 'NONE',  ( 0.000000000000000000, 8.000000000000000000, -18.50000000000000000 ) ) ;
#5507 = LINE ( 'NONE', #11782, #11093 ) ;
#5508 = ORIENTED_EDGE ( 'NONE', *, *, #4605, .F. ) ;
#5509 = DIRECTION ( 'NONE',  ( -0.000000000000000000, -1.000000000000000000, 0.000000000000000000 ) ) ;
#5510 = DIRECTION ( 'NONE',  ( 0.000000000000000000, 0.000000000000000000, 1.000000000000000000 ) ) ;
#5511 = ORIENTED_EDGE ( 'NONE', *, *, #4952, .F. ) ;
#5512 = DIRECTION ( 'NONE',  ( 6.123031769111888756E-17, 0.000000000000000000, 1.000000000000000000 ) ) ;
#5513 = ORIENTED_EDGE ( 'NONE', *, *, #7892, .F. ) ;
#5514 = PLANE ( 'NONE',  #1027 ) ;
#5515 = PLANE ( 'NONE',  #16797 ) ;
#5516 = EDGE_LOOP ( 'NONE', ( #8047, #1585, #10554, #2693 ) ) ;
#5517 = AXIS2_PLACEMENT_3D ( 'NONE', #310, #8199, #10950 ) ;
#5518 = FACE_BOUND ( 'NONE', #509, .T. ) ;
#5519 = VERTEX_POINT ( 'NONE', #3044 ) ;
#5520 = EDGE_CURVE ( 'NONE', #15647, #2162, #8194, .T. ) ;
#5521 =( NAMED_UNIT ( * ) SI_UNIT ( $, .STERADIAN. ) SOLID_ANGLE_UNIT ( ) );
#5522 = ADVANCED_FACE ( 'NONE', ( #13619 ), #12239, .F. ) ;
#5523 = LINE ( 'NONE', #13013, #7554 ) ;
#5524 = EDGE_CURVE ( 'NONE', #9064, #11889, #1844, .T. ) ;
#5525 = CLOSED_SHELL ( 'NONE', ( #15595, #4352, #4177, #363, #1762, #12767 ) ) ;
#5526 = MECHANICAL_DESIGN_GEOMETRIC_PRESENTATION_REPRESENTATION (  '', ( #16497 ), #876 ) ;
#5527 = EDGE_LOOP ( 'NONE', ( #10604, #4500, #13711, #7639 ) ) ;
#5528 = ORIENTED_EDGE ( 'NONE', *, *, #4830, .F. ) ;
#5529 = CARTESIAN_POINT ( 'NONE',  ( 35.99999999999999289, 6.000000000000000000, 17.99999999999998934 ) ) ;
#5530 = PLANE ( 'NONE',  #11547 ) ;
#5531 = DIRECTION ( 'NONE',  ( -0.000000000000000000, -1.000000000000000000, -0.000000000000000000 ) ) ;
#5532 = CIRCLE ( 'NONE', #7711, 12.50000000000001066 ) ;
#5533 = LINE ( 'NONE', #10780, #14490 ) ;
#5534 = DIRECTION ( 'NONE',  ( -1.000000000000000000, 0.000000000000000000, 0.000000000000000000 ) ) ;
#5535 = VECTOR ( 'NONE', #4168, 1000.000000000000000 ) ;
#5536 = EDGE_CURVE ( 'NONE', #11631, #2412, #16071, .T. ) ;
#5537 = DIRECTION ( 'NONE',  ( 0.000000000000000000, 0.000000000000000000, -1.000000000000000000 ) ) ;
#5538 = DIRECTION ( 'NONE',  ( 0.000000000000000000, -0.6468954956981580739, 0.7625786632508375629 ) ) ;
#5539 = AXIS2_PLACEMENT_3D ( 'NONE', #10083, #5219, #7971 ) ;
#5540 = PLANE ( 'NONE',  #10599 ) ;
#5541 = CARTESIAN_POINT ( 'NONE',  ( 30.99999999999997868, 10.00000000000000000, -30.99999999999999645 ) ) ;
#5542 = LINE ( 'NONE', #9510, #10812 ) ;
#5543 = CARTESIAN_POINT ( 'NONE',  ( -3.270000000000000462, 0.000000000000000000, 0.000000000000000000 ) ) ;
#5545 = VERTEX_POINT ( 'NONE', #7061 ) ;
#5544 = ORIENTED_EDGE ( 'NONE', *, *, #373, .F. ) ;
#5546 = CIRCLE ( 'NONE', #8298, 9.000000000000007105 ) ;
#5547 = PLANE ( 'NONE',  #977 ) ;
#5548 = CARTESIAN_POINT ( 'NONE',  ( -2.467345170754158268, 287.9032822524807216, 37.60878752180575901 ) ) ;
#5549 = VECTOR ( 'NONE', #14749, 1000.000000000000000 ) ;
#5550 = AXIS2_PLACEMENT_3D ( 'NONE', #14780, #3002, #8236 ) ;
#5551 = CARTESIAN_POINT ( 'NONE',  ( -30.99999999999999289, 68.00000000000000000, 31.00000000000000000 ) ) ;
#5552 = CARTESIAN_POINT ( 'NONE',  ( 10.00000000000000000, 481.5601199098531993, -512.1772732904406666 ) ) ;
#5553 = ORIENTED_EDGE ( 'NONE', *, *, #13805, .T. ) ;
#5554 = DIRECTION ( 'NONE',  ( 1.000000000000000000, -0.000000000000000000, 0.000000000000000000 ) ) ;
#5555 = APPLICATION_CONTEXT ( 'automotive_design' ) ;
#5556 = VECTOR ( 'NONE', #15026, 1000.000000000000000 ) ;
#5557 = LINE ( 'NONE', #9264, #15262 ) ;
#5558 = VERTEX_POINT ( 'NONE', #3141 ) ;
#5559 = DIRECTION ( 'NONE',  ( -0.9998870921963913805, -0.01502673813723916056, 0.000000000000000000 ) ) ;
#5560 = EDGE_CURVE ( 'NONE', #14313, #9254, #13059, .T. ) ;
#5561 = CARTESIAN_POINT ( 'NONE',  ( -55.99999999999989342, 559.9933750504617365, -546.7230258972048205 ) ) ;
#5562 = LINE ( 'NONE', #169, #4698 ) ;
#5563 = ORIENTED_EDGE ( 'NONE', *, *, #4094, .T. ) ;
#5564 = LINE ( 'NONE', #7879, #9136 ) ;
#5565 = AXIS2_PLACEMENT_3D ( 'NONE', #3846, #9083, #14320 ) ;
#5566 = DIRECTION ( 'NONE',  ( -1.000000000000000000, -0.000000000000000000, -0.000000000000000000 ) ) ;
#5567 = LINE ( 'NONE', #9444, #7991 ) ;
#5568 = EDGE_LOOP ( 'NONE', ( #11750, #13327, #5929, #4423 ) ) ;
#5569 = EDGE_CURVE ( 'NONE', #11572, #7931, #4343, .T. ) ;
#5570 = CARTESIAN_POINT ( 'NONE',  ( -55.99999999999989342, 523.2161522479888163, -502.8936384967199729 ) ) ;
#5571 = CIRCLE ( 'NONE', #13256, 3.300000000000025135 ) ;
#5572 = DIRECTION ( 'NONE',  ( -1.000000000000000000, 0.000000000000000000, 0.000000000000000000 ) ) ;
#5573 = CARTESIAN_POINT ( 'NONE',  ( 31.00000000000001421, 10.00000000000000000, 22.99999999999999645 ) ) ;
#5574 = ORIENTED_EDGE ( 'NONE', *, *, #14408, .T. ) ;
#5575 = VECTOR ( 'NONE', #15668, 1000.000000000000000 ) ;
#5576 = EDGE_CURVE ( 'NONE', #2891, #10664, #14815, .T. ) ;
#5577 = CIRCLE ( 'NONE', #13826, 2.999999999999999556 ) ;
#5578 = PLANE ( 'NONE',  #2524 ) ;
#5579 = DIRECTION ( 'NONE',  ( -0.000000000000000000, -0.000000000000000000, -1.000000000000000000 ) ) ;
#5580 = DIRECTION ( 'NONE',  ( -1.000000000000000000, -0.000000000000000000, -0.000000000000000000 ) ) ;
#5581 = ORIENTED_EDGE ( 'NONE', *, *, #5809, .T. ) ;
#5582 = DIRECTION ( 'NONE',  ( 1.000000000000000000, 0.000000000000000000, 0.000000000000000000 ) ) ;
#5583 = FACE_BOUND ( 'NONE', #14255, .T. ) ;
#5584 = LINE ( 'NONE', #9722, #10052 ) ;
#5585 = ORIENTED_EDGE ( 'NONE', *, *, #1546, .F. ) ;
#5586 = AXIS2_PLACEMENT_3D ( 'NONE', #11768, #5226, #3872 ) ;
#5587 = EDGE_CURVE ( 'NONE', #3136, #5238, #4421, .T. ) ;
#5588 = CARTESIAN_POINT ( 'NONE',  ( 37.50000000000000000, 196.3050121726289206, 0.000000000000000000 ) ) ;
#5589 = ORIENTED_EDGE ( 'NONE', *, *, #3322, .T. ) ;
#5590 = EDGE_LOOP ( 'NONE', ( #12670, #1564, #15806, #2849 ) ) ;
#5591 = COLOUR_RGB ( '', 0.31764706, 0.68627451, 0.89019608) ;
#5592 = CARTESIAN_POINT ( 'NONE',  ( 0.000000000000000000, 0.000000000000000000, 0.000000000000000000 ) ) ;
#5593 = VECTOR ( 'NONE', #11452, 1000.000000000000000 ) ;
#5594 = VECTOR ( 'NONE', #7216, 1000.000000000000000 ) ;
#5595 = ORIENTED_EDGE ( 'NONE', *, *, #5956, .T. ) ;
#5596 = ORIENTED_EDGE ( 'NONE', *, *, #14460, .T. ) ;
#5597 = VERTEX_POINT ( 'NONE', #5484 ) ;
#5598 = EDGE_CURVE ( 'NONE', #2603, #7648, #15250, .T. ) ;
#5599 = DIRECTION ( 'NONE',  ( 0.000000000000000000, 1.000000000000000000, 0.000000000000000000 ) ) ;
#5600 = LINE ( 'NONE', #10671, #3148 ) ;
#5601 = PRODUCT_DEFINITION_FORMATION_WITH_SPECIFIED_SOURCE ( 'ANY', '', #2443, .NOT_KNOWN. ) ;
#5602 = VERTEX_POINT ( 'NONE', #3009 ) ;
#5603 = CARTESIAN_POINT ( 'NONE',  ( 0.000000000000000000, 66.00000000000000000, -5.741599279633704455E-16 ) ) ;
#5604 = VECTOR ( 'NONE', #8699, 1000.000000000000000 ) ;
#5605 = DIRECTION ( 'NONE',  ( -1.000000000000000000, 0.000000000000000000, 0.000000000000000000 ) ) ;
#5606 = ORIENTED_EDGE ( 'NONE', *, *, #9023, .T. ) ;
#5607 = EDGE_CURVE ( 'NONE', #2250, #12986, #6947, .T. ) ;
#5608 = AXIS2_PLACEMENT_3D ( 'NONE', #11675, #10138, #3953 ) ;
#5609 = CARTESIAN_POINT ( 'NONE',  ( 1.836909530733565148E-16, 0.000000000000000000, 3.000000000000000000 ) ) ;
#5610 = EDGE_LOOP ( 'NONE', ( #1530, #2802, #7258, #1783 ) ) ;
#5611 = DIRECTION ( 'NONE',  ( -1.000000000000000000, -0.000000000000000000, -0.000000000000000000 ) ) ;
#5612 = DIRECTION ( 'NONE',  ( 0.000000000000000000, 0.000000000000000000, 1.000000000000000000 ) ) ;
#5613 = ORIENTED_EDGE ( 'NONE', *, *, #10628, .T. ) ;
#5614 = FACE_OUTER_BOUND ( 'NONE', #9592, .T. ) ;
#5615 = VERTEX_POINT ( 'NONE', #7031 ) ;
#5616 = CARTESIAN_POINT ( 'NONE',  ( 1.286622718088548112E-12, 260.4765148507136701, 287.1312267635912576 ) ) ;
#5617 = PRODUCT_DEFINITION_FORMATION_WITH_SPECIFIED_SOURCE ( 'ANY', '', #10133, .NOT_KNOWN. ) ;
#5618 = ORIENTED_EDGE ( 'NONE', *, *, #957, .F. ) ;
#5619 = VERTEX_POINT ( 'NONE', #2928 ) ;
#5620 = FACE_BOUND ( 'NONE', #9829, .T. ) ;
#5621 = ADVANCED_FACE ( 'NONE', ( #8244 ), #12032, .T. ) ;
#5622 = CIRCLE ( 'NONE', #8648, 13.69540538389601991 ) ;
#5623 = DIRECTION ( 'NONE',  ( -0.000000000000000000, -1.000000000000000000, -0.000000000000000000 ) ) ;
#5624 = DIRECTION ( 'NONE',  ( -1.000000000000000000, -0.000000000000000000, -0.000000000000000000 ) ) ;
#5625 = DIRECTION ( 'NONE',  ( -0.000000000000000000, -1.000000000000000000, -0.000000000000000000 ) ) ;
#5626 = PRODUCT_DEFINITION_SHAPE ( 'NONE', 'NONE',  #16980 ) ;
#5627 = DIRECTION ( 'NONE',  ( -0.000000000000000000, -1.000000000000000000, 0.000000000000000000 ) ) ;
#5628 = ADVANCED_FACE ( 'NONE', ( #12287 ), #13583, .T. ) ;
#5629 = ADVANCED_FACE ( 'NONE', ( #8164 ), #9545, .F. ) ;
#5630 = ADVANCED_FACE ( 'NONE', ( #7976 ), #269, .F. ) ;
#5631 = CARTESIAN_POINT ( 'NONE',  ( 5.044974746830580337, 1.808800229719332446E-15, 14.76997474683059153 ) ) ;
#5632 = EDGE_CURVE ( 'NONE', #9647, #6048, #10996, .T. ) ;
#5633 = CYLINDRICAL_SURFACE ( 'NONE', #14501, 0.7366000000000004766 ) ;
#5634 = DIRECTION ( 'NONE',  ( -0.7327934916262990317, 0.6804510993672779895, 0.000000000000000000 ) ) ;
#5635 = DIRECTION ( 'NONE',  ( 0.000000000000000000, 0.000000000000000000, -1.000000000000000000 ) ) ;
#5636 = AXIS2_PLACEMENT_3D ( 'NONE', #13298, #6654, #156 ) ;
#5637 = PLANE ( 'NONE',  #14376 ) ;
#5638 = CARTESIAN_POINT ( 'NONE',  ( 449.9999999999998295, 75.00000000000001421, 0.000000000000000000 ) ) ;
#5640 = VERTEX_POINT ( 'NONE', #2746 ) ;
#5639 = ORIENTED_EDGE ( 'NONE', *, *, #8143, .T. ) ;
#5641 = CARTESIAN_POINT ( 'NONE',  ( 2.693790225569809849, 39.66504951222130870, 9.110418847747206783 ) ) ;
#5642 = LINE ( 'NONE', #1608, #2797 ) ;
#5643 = LINE ( 'NONE', #10707, #3325 ) ;
#5644 = DIRECTION ( 'NONE',  ( 0.000000000000000000, -1.000000000000000000, -7.137148015447440312E-15 ) ) ;
#5645 = VECTOR ( 'NONE', #3288, 1000.000000000000000 ) ;
#5646 = ORIENTED_EDGE ( 'NONE', *, *, #5410, .T. ) ;
#5647 = CIRCLE ( 'NONE', #7828, 4.999999999999990230 ) ;
#5648 = CARTESIAN_POINT ( 'NONE',  ( -26.00000000000002132, 0.000000000000000000, -39.99999999999999289 ) ) ;
#5649 = EDGE_CURVE ( 'NONE', #13450, #5597, #1819, .T. ) ;
#5650 = PLANE ( 'NONE',  #14161 ) ;
#5651 = EDGE_LOOP ( 'NONE', ( #12650, #4111, #12241, #16091 ) ) ;
#5652 = FACE_OUTER_BOUND ( 'NONE', #5462, .T. ) ;
#5653 = EDGE_CURVE ( 'NONE', #7243, #13274, #14602, .T. ) ;
#5654 = CARTESIAN_POINT ( 'NONE',  ( -430.0000000000000568, 425.7506394335853201, 109.9999999999999858 ) ) ;
#5655 = DIRECTION ( 'NONE',  ( -0.000000000000000000, -1.000000000000000000, -0.000000000000000000 ) ) ;
#5656 = DIRECTION ( 'NONE',  ( -0.000000000000000000, 1.000000000000000000, -0.000000000000000000 ) ) ;
#5657 = DIRECTION ( 'NONE',  ( -1.000000000000000000, -0.000000000000000000, 0.000000000000000000 ) ) ;
#5658 = DIRECTION ( 'NONE',  ( 0.000000000000000000, 0.000000000000000000, -1.000000000000000000 ) ) ;
#5659 = ORIENTED_EDGE ( 'NONE', *, *, #170, .F. ) ;
#5660 = AXIS2_PLACEMENT_3D ( 'NONE', #4394, #13667, #9632 ) ;
#5661 = CARTESIAN_POINT ( 'NONE',  ( 394.0000000000001137, 234.3157724647196289, -110.6822657433598067 ) ) ;
#5662 = AXIS2_PLACEMENT_3D ( 'NONE', #4027, #14844, #3076 ) ;
#5663 = CARTESIAN_POINT ( 'NONE',  ( -31.00000000000002842, 0.000000000000000000, 31.00000000000000000 ) ) ;
#5664 = APPLICATION_CONTEXT ( 'automotive_design' ) ;
#5665 =( NAMED_UNIT ( * ) PLANE_ANGLE_UNIT ( ) SI_UNIT ( $, .RADIAN. ) );
#5666 = ORIENTED_EDGE ( 'NONE', *, *, #9402, .T. ) ;
#5667 = DIRECTION ( 'NONE',  ( 0.000000000000000000, 0.000000000000000000, -1.000000000000000000 ) ) ;
#5668 = UNCERTAINTY_MEASURE_WITH_UNIT (LENGTH_MEASURE( 1.000000000000000082E-05 ), #4828, 'distance_accuracy_value', 'NONE');
#5669 = CIRCLE ( 'NONE', #15273, 59.99999999999994316 ) ;
#5670 = CARTESIAN_POINT ( 'NONE',  ( 54.99999999999999289, 658.4713480608917280, -425.4301204538002139 ) ) ;
#5671 = ORIENTED_EDGE ( 'NONE', *, *, #8352, .F. ) ;
#5672 = AXIS2_PLACEMENT_3D ( 'NONE', #6534, #9304, #13090 ) ;
#5673 = CARTESIAN_POINT ( 'NONE',  ( 0.000000000000000000, 372.8685141053778693, -83.18019484660869978 ) ) ;
#5674 = CARTESIAN_POINT ( 'NONE',  ( 34.99999999999997868, 11.00000000000000000, -40.00000000000000711 ) ) ;
#5675 = FACE_OUTER_BOUND ( 'NONE', #11686, .T. ) ;
#5676 = ORIENTED_EDGE ( 'NONE', *, *, #3304, .F. ) ;
#5677 = DIRECTION ( 'NONE',  ( 0.000000000000000000, 0.000000000000000000, -1.000000000000000000 ) ) ;
#5678 = ORIENTED_EDGE ( 'NONE', *, *, #16907, .T. ) ;
#5679 = ORIENTED_EDGE ( 'NONE', *, *, #1614, .T. ) ;
#5680 = DIRECTION ( 'NONE',  ( 0.000000000000000000, 1.000000000000000000, 0.000000000000000000 ) ) ;
#5681 = ORIENTED_EDGE ( 'NONE', *, *, #14624, .F. ) ;
#5682 = CARTESIAN_POINT ( 'NONE',  ( 0.000000000000000000, 0.000000000000000000, 0.000000000000000000 ) ) ;
#5683 = AXIS2_PLACEMENT_3D ( 'NONE', #4846, #10093, #14038 ) ;
#5684 = VECTOR ( 'NONE', #2587, 1000.000000000000000 ) ;
#5685 = ORIENTED_EDGE ( 'NONE', *, *, #809, .T. ) ;
#5686 = ORIENTED_EDGE ( 'NONE', *, *, #9608, .T. ) ;
#5687 = CYLINDRICAL_SURFACE ( 'NONE', #11023, 4.000000000000000000 ) ;
#5688 = DIRECTION ( 'NONE',  ( 1.000000000000000000, -0.000000000000000000, -0.000000000000000000 ) ) ;
#5689 = ORIENTED_EDGE ( 'NONE', *, *, #5090, .T. ) ;
#5690 = LINE ( 'NONE', #10072, #9147 ) ;
#5691 = PLANE ( 'NONE',  #14741 ) ;
#5692 = EDGE_LOOP ( 'NONE', ( #5062, #16510 ) ) ;
#5693 = AXIS2_PLACEMENT_3D ( 'NONE', #13999, #469, #5696 ) ;
#5694 = PRESENTATION_STYLE_ASSIGNMENT (( #10939 ) ) ;
#5695 = EDGE_LOOP ( 'NONE', ( #7456, #662, #4015, #7294 ) ) ;
#5696 = DIRECTION ( 'NONE',  ( 0.000000000000000000, 0.000000000000000000, -1.000000000000000000 ) ) ;
#5697 = DIRECTION ( 'NONE',  ( -1.000000000000000000, -0.000000000000000000, -0.000000000000000000 ) ) ;
#5698 = EDGE_LOOP ( 'NONE', ( #7805, #8737, #5234, #8175, #4405, #7129, #14882, #181, #8773, #496, #6491, #14406, #5432, #15743, #15309, #3698, #4722, #3327, #14876, #14112, #1821, #6545, #10249, #6912, #16424, #5103, #8614, #15574 ) ) ;
#5699 = ADVANCED_FACE ( 'NONE', ( #16064 ), #16877, .T. ) ;
#5700 = VERTEX_POINT ( 'NONE', #5670 ) ;
#5701 = DIRECTION ( 'NONE',  ( -7.888609052210118054E-31, 0.000000000000000000, 1.000000000000000000 ) ) ;
#5702 = DIRECTION ( 'NONE',  ( -0.000000000000000000, -0.000000000000000000, 1.000000000000000000 ) ) ;
#5703 = ORIENTED_EDGE ( 'NONE', *, *, #5536, .F. ) ;
#5704 = AXIS2_PLACEMENT_3D ( 'NONE', #3924, #10292, #11557 ) ;
#5705 = EDGE_CURVE ( 'NONE', #5619, #5778, #2836, .T. ) ;
#5706 = VERTEX_POINT ( 'NONE', #13234 ) ;
#5707 = CYLINDRICAL_SURFACE ( 'NONE', #15961, 36.50000000000000000 ) ;
#5708 = CIRCLE ( 'NONE', #5428, 4.695405383896011919 ) ;
#5709 = DIRECTION ( 'NONE',  ( -0.000000000000000000, -1.000000000000000000, -0.000000000000000000 ) ) ;
#5710 = DIRECTION ( 'NONE',  ( 1.000000000000000000, 0.000000000000000000, 0.000000000000000000 ) ) ;
#5711 = CARTESIAN_POINT ( 'NONE',  ( -20.99999999999999645, 19.00000000000000000, -35.00000000000000711 ) ) ;
#5712 = CARTESIAN_POINT ( 'NONE',  ( 0.000000000000000000, 449.3157724647196005, -155.1251505852266632 ) ) ;
#5713 = PLANE ( 'NONE',  #2437 ) ;
#5714 = DIRECTION ( 'NONE',  ( 0.000000000000000000, -0.8660254037844379305, -0.5000000000000012212 ) ) ;
#5715 = DIRECTION ( 'NONE',  ( 0.000000000000000000, 0.000000000000000000, 1.000000000000000000 ) ) ;
#5716 = PLANE ( 'NONE',  #12693 ) ;
#5717 = ADVANCED_FACE ( 'NONE', ( #1465 ), #4215, .T. ) ;
#5718 = CARTESIAN_POINT ( 'NONE',  ( 394.0000000000001137, 449.3157724647197142, 33.76061909850716347 ) ) ;
#5719 = CIRCLE ( 'NONE', #4080, 8.000000000000000000 ) ;
#5720 = PRESENTATION_STYLE_ASSIGNMENT (( #1782 ) ) ;
#5722 = VERTEX_POINT ( 'NONE', #8331 ) ;
#5721 = ORIENTED_EDGE ( 'NONE', *, *, #11694, .T. ) ;
#5723 = CARTESIAN_POINT ( 'NONE',  ( 31.00000000000003553, 10.00000000000000000, -23.00000000000000000 ) ) ;
#5724 = EDGE_CURVE ( 'NONE', #3466, #13903, #6693, .T. ) ;
#5725 = EDGE_CURVE ( 'NONE', #11007, #9884, #11676, .T. ) ;
#5726 = SURFACE_STYLE_FILL_AREA ( #11136 ) ;
#5727 = EDGE_CURVE ( 'NONE', #16912, #2707, #10650, .T. ) ;
#5728 = CARTESIAN_POINT ( 'NONE',  ( 1.223489862255693833E-15, 380.0000000000000000, -75.00000000000000000 ) ) ;
#5729 = DIRECTION ( 'NONE',  ( -0.000000000000000000, -1.000000000000000000, 0.000000000000000000 ) ) ;
#5730 = ORIENTED_EDGE ( 'NONE', *, *, #13882, .F. ) ;
#5731 = DIRECTION ( 'NONE',  ( 0.000000000000000000, 0.000000000000000000, 1.000000000000000000 ) ) ;
#5732 = ORIENTED_EDGE ( 'NONE', *, *, #12358, .T. ) ;
#5733 = DIRECTION ( 'NONE',  ( 0.000000000000000000, -0.9848077530122090195, 0.1736481776669249744 ) ) ;
#5734 = LINE ( 'NONE', #12274, #8957 ) ;
#5735 = FACE_OUTER_BOUND ( 'NONE', #8222, .T. ) ;
#5736 = AXIS2_PLACEMENT_3D ( 'NONE', #3479, #13956, #6121 ) ;
#5737 = CARTESIAN_POINT ( 'NONE',  ( 37.50000000000000000, 196.3050121726289206, -17.00000000000000000 ) ) ;
#5738 = DIRECTION ( 'NONE',  ( 0.000000000000000000, 0.000000000000000000, 1.000000000000000000 ) ) ;
#5739 = ORIENTED_EDGE ( 'NONE', *, *, #10666, .T. ) ;
#5740 = DIRECTION ( 'NONE',  ( 0.000000000000000000, 0.9950371902099932608, -0.09950371902095787868 ) ) ;
#5741 = EDGE_CURVE ( 'NONE', #6145, #8810, #7361, .T. ) ;
#5742 = ADVANCED_FACE ( 'NONE', ( #11163, #4800 ), #3437, .F. ) ;
#5743 = DIRECTION ( 'NONE',  ( 0.000000000000000000, 0.000000000000000000, -1.000000000000000000 ) ) ;
#5744 = EDGE_CURVE ( 'NONE', #5425, #11, #3468, .T. ) ;
#5745 = DIRECTION ( 'NONE',  ( -0.000000000000000000, -1.000000000000000000, -0.000000000000000000 ) ) ;
#5746 = AXIS2_PLACEMENT_3D ( 'NONE', #6090, #11341, #16585 ) ;
#5747 = EDGE_LOOP ( 'NONE', ( #6720, #16694, #13814, #2733 ) ) ;
#5748 = DIRECTION ( 'NONE',  ( 2.920976200236518919E-15, -0.9950371902099892640, -0.09950371902099772181 ) ) ;
#5749 = DIRECTION ( 'NONE',  ( 1.000000000000000000, 1.803905316987902281E-16, 0.000000000000000000 ) ) ;
#5750 = ORIENTED_EDGE ( 'NONE', *, *, #5075, .T. ) ;
#5751 = CARTESIAN_POINT ( 'NONE',  ( -46.99999999999988631, 493.2350855268086320, -508.1801094700848580 ) ) ;
#5752 = CARTESIAN_POINT ( 'NONE',  ( 10.00000000000000000, 425.7506394335853201, 109.9999999999999858 ) ) ;
#5753 = DIRECTION ( 'NONE',  ( -1.000000000000000000, -2.911324084205185756E-15, -2.422066625794664996E-16 ) ) ;
#5754 = ORIENTED_EDGE ( 'NONE', *, *, #2398, .F. ) ;
#5755 = CARTESIAN_POINT ( 'NONE',  ( 17.00000000000000000, 380.0000000000000000, -65.00000000000000000 ) ) ;
#5756 = ORIENTED_EDGE ( 'NONE', *, *, #13051, .F. ) ;
#5757 = ORIENTED_EDGE ( 'NONE', *, *, #8624, .F. ) ;
#5758 = AXIS2_PLACEMENT_3D ( 'NONE', #5968, #3239, #655 ) ;
#5759 = LINE ( 'NONE', #9812, #12469 ) ;
#5760 = AXIS2_PLACEMENT_3D ( 'NONE', #8995, #14227, #16790 ) ;
#5761 = VERTEX_POINT ( 'NONE', #14950 ) ;
#5762 = APPLICATION_PROTOCOL_DEFINITION ( 'draft international standard', 'automotive_design', 1998, #12364 ) ;
#5763 = VECTOR ( 'NONE', #4889, 1000.000000000000000 ) ;
#5764 = EDGE_LOOP ( 'NONE', ( #5485, #1396, #7652, #11654 ) ) ;
#5765 = DIRECTION ( 'NONE',  ( -0.000000000000000000, 1.000000000000000000, -0.000000000000000000 ) ) ;
#5766 = ORIENTED_EDGE ( 'NONE', *, *, #7002, .T. ) ;
#5767 = FACE_BOUND ( 'NONE', #538, .T. ) ;
#5768 = CARTESIAN_POINT ( 'NONE',  ( -21.00000000000002842, -20.00000000000000000, -37.50000000000000000 ) ) ;
#5769 = VECTOR ( 'NONE', #2353, 1000.000000000000000 ) ;
#5770 = ORIENTED_EDGE ( 'NONE', *, *, #11071, .T. ) ;
#5772 = CARTESIAN_POINT ( 'NONE',  ( -31.00000000000002132, 0.000000000000000000, -31.00000000000000000 ) ) ;
#5771 = AXIS2_PLACEMENT_3D ( 'NONE', #2097, #739, #8287 ) ;
#5773 = CARTESIAN_POINT ( 'NONE',  ( 40.00000000000000000, 68.00000000000000000, 26.00000000000000355 ) ) ;
#5774 = ORIENTED_EDGE ( 'NONE', *, *, #8752, .T. ) ;
#5775 = DIRECTION ( 'NONE',  ( 1.000000000000000000, 0.000000000000000000, 0.000000000000000000 ) ) ;
#5776 = PRODUCT_DEFINITION_SHAPE ( 'NONE', 'NONE',  #2741 ) ;
#5777 = EDGE_CURVE ( 'NONE', #544, #1386, #9961, .T. ) ;
#5778 = VERTEX_POINT ( 'NONE', #11239 ) ;
#5779 = CARTESIAN_POINT ( 'NONE',  ( -3.270000000000000462, 285.4366476906530465, 37.52989836422091230 ) ) ;
#5780 = ORIENTED_EDGE ( 'NONE', *, *, #2381, .T. ) ;
#5781 = ORIENTED_EDGE ( 'NONE', *, *, #12665, .T. ) ;
#5782 = CARTESIAN_POINT ( 'NONE',  ( 30.90550859392621064, -45.11391548236648674, 66.87703344121217697 ) ) ;
#5783 = AXIS2_PLACEMENT_3D ( 'NONE', #16040, #4532, #16294 ) ;
#5784 = ADVANCED_FACE ( 'NONE', ( #4551, #13828 ), #8589, .T. ) ;
#5785 = ORIENTED_EDGE ( 'NONE', *, *, #998, .F. ) ;
#5786 = ORIENTED_EDGE ( 'NONE', *, *, #8528, .F. ) ;
#5787 = CARTESIAN_POINT ( 'NONE',  ( -37.00000000000000000, 0.000000000000000000, -22.99999999999999645 ) ) ;
#5788 = FACE_OUTER_BOUND ( 'NONE', #12475, .T. ) ;
#5789 = LINE ( 'NONE', #11032, #14090 ) ;
#5790 = EDGE_CURVE ( 'NONE', #4477, #3987, #12254, .T. ) ;
#5791 = DIRECTION ( 'NONE',  ( 1.000000000000000000, -0.000000000000000000, 0.000000000000000000 ) ) ;
#5792 = DIRECTION ( 'NONE',  ( 0.000000000000000000, 0.000000000000000000, 1.000000000000000000 ) ) ;
#5793 = VECTOR ( 'NONE', #13951, 1000.000000000000000 ) ;
#5794 = CARTESIAN_POINT ( 'NONE',  ( 26.00000000000000000, 19.00000000000000000, 40.00000000000001421 ) ) ;
#5795 = DIRECTION ( 'NONE',  ( 1.000000000000000000, 0.000000000000000000, 0.000000000000000000 ) ) ;
#5796 = LINE ( 'NONE', #3397, #8969 ) ;
#5797 = CARTESIAN_POINT ( 'NONE',  ( 437.7731165870194445, 329.6061121441327941, -6.736600000000000144 ) ) ;
#5798 = EDGE_CURVE ( 'NONE', #3286, #4216, #9793, .T. ) ;
#5799 = LINE ( 'NONE', #16285, #7776 ) ;
#5800 = DIRECTION ( 'NONE',  ( -3.474153781073081543E-15, -1.000000000000000000, 0.000000000000000000 ) ) ;
#5802 = EDGE_LOOP ( 'NONE', ( #12344, #2134, #3224, #7597 ) ) ;
#5801 = EDGE_LOOP ( 'NONE', ( #8599, #1067, #9097, #9210 ) ) ;
#5803 = DIRECTION ( 'NONE',  ( 0.000000000000000000, 1.000000000000000000, 0.000000000000000000 ) ) ;
#5804 = AXIS2_PLACEMENT_3D ( 'NONE', #1140, #5342, #9127 ) ;
#5805 = PLANE ( 'NONE',  #8531 ) ;
#5806 = FACE_OUTER_BOUND ( 'NONE', #2701, .T. ) ;
#5807 = ORIENTED_EDGE ( 'NONE', *, *, #3876, .F. ) ;
#5808 = AXIS2_PLACEMENT_3D ( 'NONE', #174, #3169, #9271 ) ;
#5809 = EDGE_CURVE ( 'NONE', #15912, #2740, #13070, .T. ) ;
#5810 = VECTOR ( 'NONE', #4295, 1000.000000000000000 ) ;
#5811 = PRESENTATION_LAYER_ASSIGNMENT (  '', '', ( #10470 ) ) ;
#5812 = DIRECTION ( 'NONE',  ( -1.000000000000000000, -0.000000000000000000, 0.000000000000000000 ) ) ;
#5813 = ORIENTED_EDGE ( 'NONE', *, *, #15958, .T. ) ;
#5814 = DIRECTION ( 'NONE',  ( -1.000000000000000000, 0.000000000000000000, 0.000000000000000000 ) ) ;
#5815 = CARTESIAN_POINT ( 'NONE',  ( 437.7731165870194445, 329.6061121441327941, -6.736600000000000144 ) ) ;
#5816 = CARTESIAN_POINT ( 'NONE',  ( 36.99999999999999289, 0.000000000000000000, -22.99999999999999645 ) ) ;
#5817 = CIRCLE ( 'NONE', #11570, 4.695405383896011919 ) ;
#5818 = ADVANCED_FACE ( 'NONE', ( #16398 ), #9717, .F. ) ;
#5819 = DIRECTION ( 'NONE',  ( 0.000000000000000000, 0.000000000000000000, 1.000000000000000000 ) ) ;
#5820 = CARTESIAN_POINT ( 'NONE',  ( 0.000000000000000000, 66.00000000000000000, 1.799999999999999600 ) ) ;
#5821 = EDGE_LOOP ( 'NONE', ( #12391, #14163, #16528, #8112 ) ) ;
#5822 = AXIS2_PLACEMENT_3D ( 'NONE', #680, #8663, #3335 ) ;
#5823 = CARTESIAN_POINT ( 'NONE',  ( 54.99999999999999289, 515.4878487013597805, -546.7230258972048205 ) ) ;
#5824 = VECTOR ( 'NONE', #8744, 1000.000000000000000 ) ;
#5825 = VECTOR ( 'NONE', #8715, 1000.000000000000000 ) ;
#5826 = CARTESIAN_POINT ( 'NONE',  ( -3.000000000000003109, 66.00000000000000000, 9.013878188659973034 ) ) ;
#5827 = VECTOR ( 'NONE', #11076, 1000.000000000000000 ) ;
#5828 = ORIENTED_EDGE ( 'NONE', *, *, #11399, .F. ) ;
#5829 = ADVANCED_FACE ( 'NONE', ( #6162 ), #15105, .F. ) ;
#5830 = PLANE ( 'NONE',  #14340 ) ;
#5831 = LINE ( 'NONE', #16723, #14441 ) ;
#5832 = ORIENTED_EDGE ( 'NONE', *, *, #14271, .T. ) ;
#5833 = CARTESIAN_POINT ( 'NONE',  ( 10.00000000000000000, 226.8713558223388134, -346.2582248962859808 ) ) ;
#5834 = CIRCLE ( 'NONE', #16262, 6.473199999999998511 ) ;
#5835 = VECTOR ( 'NONE', #9621, 1000.000000000000000 ) ;
#5836 = EDGE_CURVE ( 'NONE', #748, #14972, #5098, .T. ) ;
#5837 = DIRECTION ( 'NONE',  ( -0.000000000000000000, -0.000000000000000000, 1.000000000000000000 ) ) ;
#5838 = PLANE ( 'NONE',  #3742 ) ;
#5839 = VERTEX_POINT ( 'NONE', #12534 ) ;
#5840 = EDGE_CURVE ( 'NONE', #7396, #1879, #13912, .T. ) ;
#5841 = EDGE_CURVE ( 'NONE', #9546, #717, #14716, .T. ) ;
#5842 = EDGE_CURVE ( 'NONE', #8810, #1911, #10600, .T. ) ;
#5843 = SHAPE_REPRESENTATION ( 'Servo-Body', ( #1488 ), #3145 ) ;
#5844 = EDGE_LOOP ( 'NONE', ( #4585, #1672, #14698, #4158, #11178 ) ) ;
#5845 = ORIENTED_EDGE ( 'NONE', *, *, #6632, .T. ) ;
#5846 = CARTESIAN_POINT ( 'NONE',  ( 10.00000000000000000, 435.2933666400819561, -525.1288175801793159 ) ) ;
#5847 = VECTOR ( 'NONE', #10262, 1000.000000000000000 ) ;
#5848 = CIRCLE ( 'NONE', #1460, 4.695405383895955964 ) ;
#5849 = AXIS2_PLACEMENT_3D ( 'NONE', #6979, #5697, #14891 ) ;
#5850 = VECTOR ( 'NONE', #14394, 1000.000000000000000 ) ;
#5851 = CARTESIAN_POINT ( 'NONE',  ( 0.000000000000000000, 0.000000000000000000, 0.000000000000000000 ) ) ;
#5852 = VERTEX_POINT ( 'NONE', #3186 ) ;
#5853 = CYLINDRICAL_SURFACE ( 'NONE', #12938, 10.00000000000000178 ) ;
#5854 = FACE_OUTER_BOUND ( 'NONE', #9151, .T. ) ;
#5855 = VECTOR ( 'NONE', #719, 1000.000000000000000 ) ;
#5856 = EDGE_LOOP ( 'NONE', ( #11115, #14790, #5225, #1845 ) ) ;
#5857 = CARTESIAN_POINT ( 'NONE',  ( -20.00000000000003197, 0.000000000000000000, 40.00000000000000711 ) ) ;
#5858 = DIRECTION ( 'NONE',  ( 0.000000000000000000, -1.000000000000000000, 0.000000000000000000 ) ) ;
#5859 = EDGE_LOOP ( 'NONE', ( #11537, #10237, #10919, #10160 ) ) ;
#5860 = AXIS2_PLACEMENT_3D ( 'NONE', #9327, #5534, #8286 ) ;
#5861 = EDGE_CURVE ( 'NONE', #4858, #16000, #13663, .T. ) ;
#5862 = CARTESIAN_POINT ( 'NONE',  ( 35.00000000000003553, 3.000000000000000000, -20.99999999999999645 ) ) ;
#5863 = VERTEX_POINT ( 'NONE', #12368 ) ;
#5864 = EDGE_LOOP ( 'NONE', ( #11608, #14471, #5868, #6315 ) ) ;
#5865 = VERTEX_POINT ( 'NONE', #606 ) ;
#5867 = CIRCLE ( 'NONE', #12458, 3.999999999999996447 ) ;
#5866 = ADVANCED_BREP_SHAPE_REPRESENTATION ( '', ( #8939, #3183, #1488 ), #3972 ) ;
#5868 = ORIENTED_EDGE ( 'NONE', *, *, #66, .F. ) ;
#5869 = PRESENTATION_LAYER_ASSIGNMENT (  '', '', ( #13291 ) ) ;
#5870 = EDGE_LOOP ( 'NONE', ( #15585, #6628 ) ) ;
#5872 = LINE ( 'NONE', #11117, #15687 ) ;
#5871 =( GEOMETRIC_REPRESENTATION_CONTEXT ( 3 ) GLOBAL_UNCERTAINTY_ASSIGNED_CONTEXT ( ( #1716 ) ) GLOBAL_UNIT_ASSIGNED_CONTEXT ( ( #13062, #7800, #14430 ) ) REPRESENTATION_CONTEXT ( 'NONE', 'WORKASPACE' ) );
#5873 = AXIS2_PLACEMENT_3D ( 'NONE', #4639, #15044, #1986 ) ;
#5874 = EDGE_CURVE ( 'NONE', #5640, #1911, #5831, .T. ) ;
#5875 = PLANE ( 'NONE',  #2508 ) ;
#5876 = PLANE ( 'NONE',  #11339 ) ;
#5877 = DIRECTION ( 'NONE',  ( 0.000000000000000000, 0.000000000000000000, 1.000000000000000000 ) ) ;
#5878 = TOROIDAL_SURFACE ( 'NONE', #14391, 4.695405383895982609, 9.000000000000000000 ) ;
#5879 = DIRECTION ( 'NONE',  ( 1.000000000000000000, 0.000000000000000000, 0.000000000000000000 ) ) ;
#5880 = FACE_OUTER_BOUND ( 'NONE', #7699, .T. ) ;
#5881 = LINE ( 'NONE', #12496, #7135 ) ;
#5882 = EDGE_LOOP ( 'NONE', ( #16218, #10973, #12038, #7279 ) ) ;
#5883 = FACE_OUTER_BOUND ( 'NONE', #16005, .T. ) ;
#5884 = DIRECTION ( 'NONE',  ( 0.000000000000000000, 0.8660254037844424824, -0.4999999999999933387 ) ) ;
#5885 = PRODUCT_DEFINITION_FORMATION_WITH_SPECIFIED_SOURCE ( 'ANY', '', #8239, .NOT_KNOWN. ) ;
#5886 = DIRECTION ( 'NONE',  ( 0.000000000000000000, 0.000000000000000000, -1.000000000000000000 ) ) ;
#5887 = CIRCLE ( 'NONE', #1505, 4.695405383896011919 ) ;
#5888 = PLANE ( 'NONE',  #3298 ) ;
#5890 = ORIENTED_EDGE ( 'NONE', *, *, #9670, .T. ) ;
#5889 = ORIENTED_EDGE ( 'NONE', *, *, #16493, .T. ) ;
#5891 = CARTESIAN_POINT ( 'NONE',  ( 2.383743612111322463, 39.16804506571254763, 9.196765735797566066 ) ) ;
#5892 = VECTOR ( 'NONE', #4036, 1000.000000000000000 ) ;
#5893 = ITEM_DEFINED_TRANSFORMATION ( 'NONE', 'NONE', #12999,  #1488 ) ;
#5894 = VERTEX_POINT ( 'NONE', #7617 ) ;
#5895 =( LENGTH_UNIT ( ) NAMED_UNIT ( * ) SI_UNIT ( .MILLI., .METRE. ) );
#5896 = DIRECTION ( 'NONE',  ( 0.000000000000000000, 0.000000000000000000, 1.000000000000000000 ) ) ;
#5897 = CARTESIAN_POINT ( 'NONE',  ( 30.99999999999999645, 3.000000000000000000, -25.99999999999999645 ) ) ;
#5898 = VERTEX_POINT ( 'NONE', #2557 ) ;
#5899 = DIRECTION ( 'NONE',  ( 0.000000000000000000, 0.000000000000000000, -1.000000000000000000 ) ) ;
#5900 = CARTESIAN_POINT ( 'NONE',  ( -31.00000000000006395, 3.000000000000000000, -25.99999999999999645 ) ) ;
#5901 = CARTESIAN_POINT ( 'NONE',  ( 31.00000000000000000, 19.00000000000000000, -31.00000000000000355 ) ) ;
#5902 = ORIENTED_EDGE ( 'NONE', *, *, #13843, .F. ) ;
#5903 = DIRECTION ( 'NONE',  ( 0.000000000000000000, 0.000000000000000000, 1.000000000000000000 ) ) ;
#5904 = AXIS2_PLACEMENT_3D ( 'NONE', #13964, #910, #10099 ) ;
#5905 = CARTESIAN_POINT ( 'NONE',  ( 0.1475654038909327559, 193.0227741332293192, 37.40882805463644445 ) ) ;
#5906 = DIRECTION ( 'NONE',  ( 1.000000000000000000, 0.000000000000000000, 0.000000000000000000 ) ) ;
#5907 = PRODUCT_DEFINITION_SHAPE ( 'NONE', 'NONE',  #16977 ) ;
#5908 = DIRECTION ( 'NONE',  ( 1.000000000000000000, 0.000000000000000000, 0.000000000000000000 ) ) ;
#5909 = LINE ( 'NONE', #4786, #16394 ) ;
#5910 = ORIENTED_EDGE ( 'NONE', *, *, #5607, .F. ) ;
#5911 = DIRECTION ( 'NONE',  ( 0.000000000000000000, 0.000000000000000000, 1.000000000000000000 ) ) ;
#5912 = EDGE_CURVE ( 'NONE', #12736, #9686, #13128, .T. ) ;
#5913 = VECTOR ( 'NONE', #6984, 1000.000000000000000 ) ;
#5914 = ORIENTED_EDGE ( 'NONE', *, *, #15357, .F. ) ;
#5915 = LINE ( 'NONE', #4702, #3915 ) ;
#5916 = EDGE_CURVE ( 'NONE', #197, #5152, #9505, .T. ) ;
#5917 = VERTEX_POINT ( 'NONE', #15536 ) ;
#5918 = DIRECTION ( 'NONE',  ( 0.000000000000000000, -1.000000000000000000, 0.000000000000000000 ) ) ;
#5919 = DIRECTION ( 'NONE',  ( 1.000000000000000000, -0.000000000000000000, 0.000000000000000000 ) ) ;
#5920 = VERTEX_POINT ( 'NONE', #2466 ) ;
#5921 = DIRECTION ( 'NONE',  ( 0.000000000000000000, 0.000000000000000000, -1.000000000000000000 ) ) ;
#5922 = CARTESIAN_POINT ( 'NONE',  ( 10.00000000000000000, 1.106257942394396377E-12, -155.0000000000060254 ) ) ;
#5923 = FACE_OUTER_BOUND ( 'NONE', #13338, .T. ) ;
#5924 = ORIENTED_EDGE ( 'NONE', *, *, #4581, .F. ) ;
#5925 = AXIS2_PLACEMENT_3D ( 'NONE', #11168, #12708, #10131 ) ;
#5926 = AXIS2_PLACEMENT_3D ( 'NONE', #13741, #5919, #16565 ) ;
#5927 = DIRECTION ( 'NONE',  ( 0.000000000000000000, 0.000000000000000000, -1.000000000000000000 ) ) ;
#5928 = VERTEX_POINT ( 'NONE', #3687 ) ;
#5929 = ORIENTED_EDGE ( 'NONE', *, *, #2784, .T. ) ;
#5930 = CARTESIAN_POINT ( 'NONE',  ( -55.99999999999989342, 559.9933750504617365, -551.4184312811007658 ) ) ;
#5931 = EDGE_CURVE ( 'NONE', #12617, #4130, #6456, .T. ) ;
#5932 = SHAPE_DEFINITION_REPRESENTATION ( #13598, #135 ) ;
#5933 = ADVANCED_FACE ( 'NONE', ( #11414 ), #11687, .F. ) ;
#5934 = CARTESIAN_POINT ( 'NONE',  ( 31.00000000000003908, 19.00000000000000000, -26.00000000000000355 ) ) ;
#5935 = EDGE_CURVE ( 'NONE', #9768, #5545, #4879, .T. ) ;
#5936 = ADVANCED_FACE ( 'NONE', ( #5129 ), #10380, .T. ) ;
#5937 = ORIENTED_EDGE ( 'NONE', *, *, #11588, .T. ) ;
#5938 = CIRCLE ( 'NONE', #8959, 2.500000000000002220 ) ;
#5939 = EDGE_CURVE ( 'NONE', #9126, #16083, #9086, .T. ) ;
#5940 = LINE ( 'NONE', #7215, #9931 ) ;
#5941 = CARTESIAN_POINT ( 'NONE',  ( 0.000000000000000000, 376.0487089519832011, -80.00000000000332534 ) ) ;
#5942 = VERTEX_POINT ( 'NONE', #14247 ) ;
#5943 = CARTESIAN_POINT ( 'NONE',  ( 65.00000000000000000, 380.0000000000000000, -17.00000000000000355 ) ) ;
#5944 = CYLINDRICAL_SURFACE ( 'NONE', #7012, 2.500000000000002220 ) ;
#5945 = ORIENTED_EDGE ( 'NONE', *, *, #4563, .F. ) ;
#5946 = CARTESIAN_POINT ( 'NONE',  ( 0.7365999999999783832, 260.4765148507123058, 287.1312267635911439 ) ) ;
#5947 = ORIENTED_EDGE ( 'NONE', *, *, #6107, .T. ) ;
#5948 = ORIENTED_EDGE ( 'NONE', *, *, #7298, .T. ) ;
#5949 = AXIS2_PLACEMENT_3D ( 'NONE', #8802, #986, #16687 ) ;
#5950 = AXIS2_PLACEMENT_3D ( 'NONE', #12731, #9988, #8779 ) ;
#5951 = ORIENTED_EDGE ( 'NONE', *, *, #6579, .F. ) ;
#5952 = ORIENTED_EDGE ( 'NONE', *, *, #12746, .T. ) ;
#5953 = ADVANCED_FACE ( 'NONE', ( #11663 ), #14325, .F. ) ;
#5954 = ORIENTED_EDGE ( 'NONE', *, *, #16418, .F. ) ;
#5955 = CARTESIAN_POINT ( 'NONE',  ( -1.831162533324883990, 38.61573685184089300, 9.323294315095141727 ) ) ;
#5956 = EDGE_CURVE ( 'NONE', #6058, #9277, #14996, .T. ) ;
#5957 = DIRECTION ( 'NONE',  ( -0.000000000000000000, 1.000000000000000000, -0.000000000000000000 ) ) ;
#5958 = LINE ( 'NONE', #16761, #8055 ) ;
#5959 = DIRECTION ( 'NONE',  ( 1.000000000000000000, 0.000000000000000000, -0.000000000000000000 ) ) ;
#5960 = CARTESIAN_POINT ( 'NONE',  ( 34.99999999999997868, 0.000000000000000000, -40.00000000000000711 ) ) ;
#5961 = CARTESIAN_POINT ( 'NONE',  ( 10.00000000000000000, 396.9484440344699010, -165.7668752622531088 ) ) ;
#5962 = CARTESIAN_POINT ( 'NONE',  ( 0.7365999999999927050, 189.4632308570089094, 37.52989836422091940 ) ) ;
#5963 = FACE_BOUND ( 'NONE', #10658, .T. ) ;
#5964 = ORIENTED_EDGE ( 'NONE', *, *, #7679, .F. ) ;
#5965 = DIRECTION ( 'NONE',  ( 0.000000000000000000, 0.000000000000000000, -1.000000000000000000 ) ) ;
#5966 = CARTESIAN_POINT ( 'NONE',  ( 0.000000000000000000, 234.3157724647196289, -110.6822657433598067 ) ) ;
#5967 = DIRECTION ( 'NONE',  ( -1.000000000000000000, -0.000000000000000000, 0.000000000000000000 ) ) ;
#5968 = CARTESIAN_POINT ( 'NONE',  ( -10.00000000000000000, 0.000000000000000000, 0.000000000000000000 ) ) ;
#5969 = EDGE_CURVE ( 'NONE', #2075, #884, #1273, .T. ) ;
#5971 = ORIENTED_EDGE ( 'NONE', *, *, #6981, .F. ) ;
#5970 = EDGE_LOOP ( 'NONE', ( #698, #208, #10419, #8954 ) ) ;
#5972 = CIRCLE ( 'NONE', #10923, 4.695405383896011919 ) ;
#5973 = LINE ( 'NONE', #11048, #15778 ) ;
#5974 = FILL_AREA_STYLE_COLOUR ( '', #13761 ) ;
#5975 = DIRECTION ( 'NONE',  ( 1.000000000000000000, -0.000000000000000000, -0.000000000000000000 ) ) ;
#5976 = CARTESIAN_POINT ( 'NONE',  ( -18.00000000000000711, 0.000000000000000000, -5.268482129199949959 ) ) ;
#5977 = EDGE_LOOP ( 'NONE', ( #2999, #15317, #3382, #12755 ) ) ;
#5978 = DIRECTION ( 'NONE',  ( 0.000000000000000000, 0.000000000000000000, 1.000000000000000000 ) ) ;
#5979 = CARTESIAN_POINT ( 'NONE',  ( -23.00000000000002487, 0.000000000000000000, -36.99999999999999289 ) ) ;
#5980 = VERTEX_POINT ( 'NONE', #6490 ) ;
#5981 = FACE_OUTER_BOUND ( 'NONE', #10856, .T. ) ;
#5982 = LINE ( 'NONE', #12686, #1961 ) ;
#5983 = CARTESIAN_POINT ( 'NONE',  ( -23.00000000000002132, 10.00000000000000000, 37.00000000000000711 ) ) ;
#5984 = CARTESIAN_POINT ( 'NONE',  ( 55.99999999999989342, 493.2350855268092573, -598.9613477082210693 ) ) ;
#5985 = EDGE_LOOP ( 'NONE', ( #1335, #13668, #16117, #15020 ) ) ;
#5986 = CARTESIAN_POINT ( 'NONE',  ( 21.00000000000000000, 8.000000000000000000, 35.00000000000001421 ) ) ;
#5987 = DIRECTION ( 'NONE',  ( -0.000000000000000000, 1.000000000000000000, -0.000000000000000000 ) ) ;
#5988 = ORIENTED_EDGE ( 'NONE', *, *, #10444, .F. ) ;
#5989 = FILL_AREA_STYLE ('',( #2047 ) ) ;
#5990 = ORIENTED_EDGE ( 'NONE', *, *, #16207, .T. ) ;
#5991 = FACE_BOUND ( 'NONE', #8475, .T. ) ;
#5992 = EDGE_CURVE ( 'NONE', #1375, #7813, #9235, .T. ) ;
#5993 = CARTESIAN_POINT ( 'NONE',  ( -31.81980515339462912, 11.00000000000000000, 31.81980515339465043 ) ) ;
#5994 = VERTEX_POINT ( 'NONE', #3939 ) ;
#5995 = CARTESIAN_POINT ( 'NONE',  ( -46.99999999999988631, 523.2161522479893847, -590.5524132976893270 ) ) ;
#5996 = CARTESIAN_POINT ( 'NONE',  ( 30.99999999999995737, 3.000000000000000000, 31.00000000000000000 ) ) ;
#5997 = PLANE ( 'NONE',  #16625 ) ;
#5998 = EDGE_LOOP ( 'NONE', ( #7116, #1968, #13120, #1118 ) ) ;
#5999 = CARTESIAN_POINT ( 'NONE',  ( -5.000000000000000888, 0.000000000000000000, 22.46376988133006236 ) ) ;
#6000 = FILL_AREA_STYLE_COLOUR ( '', #7324 ) ;
#6001 = ORIENTED_EDGE ( 'NONE', *, *, #10017, .T. ) ;
#6002 = ORIENTED_EDGE ( 'NONE', *, *, #10058, .F. ) ;
#6003 = ADVANCED_FACE ( 'NONE', ( #9011 ), #8377, .F. ) ;
#6004 = DIRECTION ( 'NONE',  ( -1.000000000000000000, 0.000000000000000000, 0.000000000000000000 ) ) ;
#6005 = APPLICATION_PROTOCOL_DEFINITION ( 'draft international standard', 'automotive_design', 1998, #4781 ) ;
#6006 = VECTOR ( 'NONE', #9357, 1000.000000000000114 ) ;
#6007 = FACE_OUTER_BOUND ( 'NONE', #3765, .T. ) ;
#6008 = ORIENTED_EDGE ( 'NONE', *, *, #7180, .F. ) ;
#6009 = CARTESIAN_POINT ( 'NONE',  ( 55.99999999999989342, 549.5810598491749488, -580.0260321808809749 ) ) ;
#6010 = CARTESIAN_POINT ( 'NONE',  ( -40.00000000000000000, 19.00000000000000000, 25.99999999999999645 ) ) ;
#6011 = EDGE_CURVE ( 'NONE', #6668, #10633, #2086, .T. ) ;
#6012 = ORIENTED_EDGE ( 'NONE', *, *, #11673, .T. ) ;
#6013 = DIRECTION ( 'NONE',  ( -4.956352788505164254E-16, 0.000000000000000000, 1.000000000000000000 ) ) ;
#6014 = EDGE_CURVE ( 'NONE', #9484, #985, #4302, .T. ) ;
#6015 = DIRECTION ( 'NONE',  ( -0.000000000000000000, -1.000000000000000000, 0.000000000000000000 ) ) ;
#6016 = ORIENTED_EDGE ( 'NONE', *, *, #7829, .T. ) ;
#6017 = VECTOR ( 'NONE', #3400, 1000.000000000000000 ) ;
#6018 = CARTESIAN_POINT ( 'NONE',  ( -46.99999999999988631, 549.5810598491749488, -561.6352214130889706 ) ) ;
#6019 = ADVANCED_FACE ( 'NONE', ( #14073 ), #7533, .T. ) ;
#6020 = ORIENTED_EDGE ( 'NONE', *, *, #2425, .F. ) ;
#6021 = ORIENTED_EDGE ( 'NONE', *, *, #15506, .T. ) ;
#6022 = EDGE_CURVE ( 'NONE', #11607, #6185, #11420, .T. ) ;
#6023 = EDGE_CURVE ( 'NONE', #7810, #9524, #5557, .T. ) ;
#6024 = ORIENTED_EDGE ( 'NONE', *, *, #6038, .T. ) ;
#6025 = VERTEX_POINT ( 'NONE', #10806 ) ;
#6026 = AXIS2_PLACEMENT_3D ( 'NONE', #9236, #15911, #13445 ) ;
#6027 = EDGE_LOOP ( 'NONE', ( #16776, #12729, #13319, #16243, #5416 ) ) ;
#6028 = CARTESIAN_POINT ( 'NONE',  ( -1.507804506096813046, 38.39915541515519237, 9.381017998102995747 ) ) ;
#6029 = AXIS2_PLACEMENT_3D ( 'NONE', #80, #5467, #4373 ) ;
#6030 = CARTESIAN_POINT ( 'NONE',  ( 1.399999999999999911, 0.000000000000000000, 0.000000000000000000 ) ) ;
#6031 = LINE ( 'NONE', #8632, #1477 ) ;
#6032 = EDGE_CURVE ( 'NONE', #3717, #14752, #4370, .T. ) ;
#6033 = CARTESIAN_POINT ( 'NONE',  ( -20.99999999999999645, 8.000000000000000000, 31.00000000000003197 ) ) ;
#6034 = DIRECTION ( 'NONE',  ( 1.000000000000000000, -0.000000000000000000, 0.000000000000000000 ) ) ;
#6035 = DIRECTION ( 'NONE',  ( -0.000000000000000000, -1.000000000000000000, -0.000000000000000000 ) ) ;
#6036 = DIRECTION ( 'NONE',  ( 0.000000000000000000, -0.000000000000000000, 1.000000000000000000 ) ) ;
#6037 = LINE ( 'NONE', #9840, #1339 ) ;
#6038 = EDGE_CURVE ( 'NONE', #7123, #1069, #422, .T. ) ;
#6039 = ORIENTED_EDGE ( 'NONE', *, *, #3943, .F. ) ;
#6040 = CARTESIAN_POINT ( 'NONE',  ( -13.11912225705329327, 0.000000000000000000, 0.000000000000000000 ) ) ;
#6041 = LINE ( 'NONE', #7410, #15436 ) ;
#6042 = ADVANCED_FACE ( 'NONE', ( #16044 ), #5650, .F. ) ;
#6043 = CIRCLE ( 'NONE', #16205, 9.000000000000007105 ) ;
#6044 = EDGE_CURVE ( 'NONE', #6110, #6925, #8685, .T. ) ;
#6045 = ADVANCED_FACE ( 'NONE', ( #5386 ), #15863, .F. ) ;
#6046 = CYLINDRICAL_SURFACE ( 'NONE', #15900, 84.99999999999997158 ) ;
#6048 = VERTEX_POINT ( 'NONE', #1533 ) ;
#6047 = EDGE_LOOP ( 'NONE', ( #15814, #16227, #11550, #7320 ) ) ;
#6049 = DIRECTION ( 'NONE',  ( 0.000000000000000000, 1.000000000000000000, 0.000000000000000000 ) ) ;
#6050 = FACE_OUTER_BOUND ( 'NONE', #12305, .T. ) ;
#6051 = DIRECTION ( 'NONE',  ( -1.000000000000000000, 0.000000000000000000, -0.000000000000000000 ) ) ;
#6052 = CARTESIAN_POINT ( 'NONE',  ( 39.99999999999999289, 8.000000000000000000, 26.00000000000000000 ) ) ;
#6053 = CONICAL_SURFACE ( 'NONE', #14024, 18.17500000000000071, 0.7483780475235185525 ) ;
#6054 = VERTEX_POINT ( 'NONE', #6924 ) ;
#6055 = UNCERTAINTY_MEASURE_WITH_UNIT (LENGTH_MEASURE( 1.000000000000000082E-05 ), #1412, 'distance_accuracy_value', 'NONE');
#6056 = DIRECTION ( 'NONE',  ( -1.000000000000000000, -6.123031769111888756E-17, 6.123031769111888756E-17 ) ) ;
#6057 = LINE ( 'NONE', #11304, #16094 ) ;
#6058 = VERTEX_POINT ( 'NONE', #2988 ) ;
#6059 = CARTESIAN_POINT ( 'NONE',  ( -55.99999999999989342, 559.9933750504617365, -546.7230258972048205 ) ) ;
#6060 = CARTESIAN_POINT ( 'NONE',  ( 0.09296894633975227862, 193.1074002614837468, 37.43392030153066230 ) ) ;
#6061 = CYLINDRICAL_SURFACE ( 'NONE', #3087, 7.999999999999996447 ) ;
#6062 = CARTESIAN_POINT ( 'NONE',  ( 45.00000000000000000, 559.9933750504617365, -560.4184312811007658 ) ) ;
#6063 = LINE ( 'NONE', #16553, #9554 ) ;
#6064 = ORIENTED_EDGE ( 'NONE', *, *, #9828, .F. ) ;
#6065 = CIRCLE ( 'NONE', #1955, 9.000000000000007105 ) ;
#6066 = DIRECTION ( 'NONE',  ( 0.000000000000000000, 0.000000000000000000, 1.000000000000000000 ) ) ;
#6067 = LINE ( 'NONE', #6156, #7651 ) ;
#6068 = AXIS2_PLACEMENT_3D ( 'NONE', #7878, #13133, #1360 ) ;
#6069 = ORIENTED_EDGE ( 'NONE', *, *, #3216, .T. ) ;
#6070 = SURFACE_STYLE_USAGE ( .BOTH. , #3344 ) ;
#6071 = ORIENTED_EDGE ( 'NONE', *, *, #1524, .F. ) ;
#6072 = FACE_OUTER_BOUND ( 'NONE', #12960, .T. ) ;
#6073 = EDGE_CURVE ( 'NONE', #13726, #2088, #8309, .T. ) ;
#6074 = DIRECTION ( 'NONE',  ( 0.000000000000000000, -1.850371707708599493E-15, -1.000000000000000000 ) ) ;
#6075 = ORIENTED_EDGE ( 'NONE', *, *, #16540, .T. ) ;
#6076 = DIRECTION ( 'NONE',  ( -0.000000000000000000, 1.000000000000000000, -0.000000000000000000 ) ) ;
#6077 = CARTESIAN_POINT ( 'NONE',  ( 22.99999999999998224, 6.000000000000000000, -36.99999999999999289 ) ) ;
#6078 = CARTESIAN_POINT ( 'NONE',  ( 0.000000000000000000, 226.8713558223388134, -358.7582248962859808 ) ) ;
#6079 = ORIENTED_EDGE ( 'NONE', *, *, #6742, .F. ) ;
#6080 = EDGE_CURVE ( 'NONE', #12484, #14967, #8221, .T. ) ;
#6081 = VECTOR ( 'NONE', #7267, 1000.000000000000000 ) ;
#6082 = AXIS2_PLACEMENT_3D ( 'NONE', #9152, #12763, #10278 ) ;
#6083 = DIRECTION ( 'NONE',  ( -0.000000000000000000, -0.000000000000000000, 1.000000000000000000 ) ) ;
#6084 = CARTESIAN_POINT ( 'NONE',  ( -2.467345170754123185, 287.9032822524808353, 37.60878752180576612 ) ) ;
#6085 = ORIENTED_EDGE ( 'NONE', *, *, #8064, .T. ) ;
#6086 = ORIENTED_EDGE ( 'NONE', *, *, #2696, .T. ) ;
#6087 = DIRECTION ( 'NONE',  ( -0.000000000000000000, 1.000000000000000000, -0.000000000000000000 ) ) ;
#6088 = PRODUCT_CONTEXT ( 'NONE', #10935, 'mechanical' ) ;
#6089 = AXIS2_PLACEMENT_3D ( 'NONE', #12110, #3095, #5481 ) ;
#6090 = CARTESIAN_POINT ( 'NONE',  ( -22.99999999999999645, 68.00000000000000000, 37.00000000000002132 ) ) ;
#6091 = ORIENTED_EDGE ( 'NONE', *, *, #4867, .T. ) ;
#6092 = CIRCLE ( 'NONE', #355, 3.300000000000011369 ) ;
#6093 = DIRECTION ( 'NONE',  ( -1.000000000000000000, -0.000000000000000000, 0.000000000000000000 ) ) ;
#6094 = CARTESIAN_POINT ( 'NONE',  ( 394.0000000000001137, 449.3157724647196005, -155.1251505852266632 ) ) ;
#6095 = ADVANCED_FACE ( 'NONE', ( #5296, #12185 ), #10897, .F. ) ;
#6096 = ORIENTED_EDGE ( 'NONE', *, *, #14332, .T. ) ;
#6097 = PLANE ( 'NONE',  #6384 ) ;
#6098 = DIRECTION ( 'NONE',  ( 0.000000000000000000, 0.09950371902098545385, -0.9950371902099903743 ) ) ;
#6099 = ORIENTED_EDGE ( 'NONE', *, *, #2534, .T. ) ;
#6100 = AXIS2_PLACEMENT_3D ( 'NONE', #7784, #6316, #2465 ) ;
#6101 = ORIENTED_EDGE ( 'NONE', *, *, #9929, .T. ) ;
#6102 = ORIENTED_EDGE ( 'NONE', *, *, #16637, .T. ) ;
#6103 = CIRCLE ( 'NONE', #12705, 13.69540538389601991 ) ;
#6104 = AXIS2_PLACEMENT_3D ( 'NONE', #3071, #8305, #3167 ) ;
#6105 = ORIENTED_EDGE ( 'NONE', *, *, #2234, .F. ) ;
#6106 = SHAPE_REPRESENTATION_RELATIONSHIP ( 'NONE' , 'NONE' ,  #1883, #12020 ) ;
#6107 = EDGE_CURVE ( 'NONE', #9290, #14252, #11831, .T. ) ;
#6108 = ORIENTED_EDGE ( 'NONE', *, *, #2360, .F. ) ;
#6109 = VECTOR ( 'NONE', #2605, 1000.000000000000114 ) ;
#6110 = VERTEX_POINT ( 'NONE', #2725 ) ;
#6111 = LINE ( 'NONE', #12365, #14606 ) ;
#6112 = CARTESIAN_POINT ( 'NONE',  ( 0.6999999999999999556, 0.000000000000000000, 0.000000000000000000 ) ) ;
#6113 = PLANE ( 'NONE',  #10258 ) ;
#6114 = AXIS2_PLACEMENT_3D ( 'NONE', #16671, #4905, #10155 ) ;
#6115 = ADVANCED_FACE ( 'NONE', ( #6576 ), #10547, .T. ) ;
#6116 = AXIS2_PLACEMENT_3D ( 'NONE', #16765, #11621, #4918 ) ;
#6117 = CYLINDRICAL_SURFACE ( 'NONE', #14779, 3.300000000000025135 ) ;
#6118 = CARTESIAN_POINT ( 'NONE',  ( 6.117449311278470645E-17, 355.3192028797624857, -44.71049682360899169 ) ) ;
#6119 = AXIS2_PLACEMENT_3D ( 'NONE', #15925, #8200, #2706 ) ;
#6120 = CARTESIAN_POINT ( 'NONE',  ( 31.00000000000002842, 68.00000000000000000, 23.00000000000001066 ) ) ;
#6121 = DIRECTION ( 'NONE',  ( 0.000000000000000000, 0.000000000000000000, -1.000000000000000000 ) ) ;
#6122 = CARTESIAN_POINT ( 'NONE',  ( 10.00000000000000000, 185.0000000000000568, -1.831360450120427585E-14 ) ) ;
#6123 = ORIENTED_EDGE ( 'NONE', *, *, #2247, .F. ) ;
#6124 = CARTESIAN_POINT ( 'NONE',  ( 18.99999999999998224, 8.000000000000000000, -39.99999999999999289 ) ) ;
#6125 = CARTESIAN_POINT ( 'NONE',  ( -31.81980515339462912, 8.000000000000000000, -35.11980515339465114 ) ) ;
#6126 = AXIS2_PLACEMENT_3D ( 'NONE', #2325, #14265, #1376 ) ;
#6127 = CARTESIAN_POINT ( 'NONE',  ( 56.72999999999999687, 214.4632308570087957, 287.5298983642209123 ) ) ;
#6129 = ORIENTED_EDGE ( 'NONE', *, *, #16445, .F. ) ;
#6128 = VERTEX_POINT ( 'NONE', #7959 ) ;
#6130 = AXIS2_PLACEMENT_3D ( 'NONE', #2668, #4051, #10738 ) ;
#6131 = CARTESIAN_POINT ( 'NONE',  ( -20.99999999999999645, 19.00000000000000000, 31.00000000000003197 ) ) ;
#6132 = EDGE_CURVE ( 'NONE', #14475, #10621, #11142, .T. ) ;
#6133 = ORIENTED_EDGE ( 'NONE', *, *, #9023, .F. ) ;
#6134 = AXIS2_PLACEMENT_3D ( 'NONE', #8033, #6743, #16031 ) ;
#6135 = CARTESIAN_POINT ( 'NONE',  ( 17.00000000000000711, 355.3192028797624857, -29.71049682360898814 ) ) ;
#6136 = ADVANCED_FACE ( 'NONE', ( #1444 ), #6672, .F. ) ;
#6137 = DIRECTION ( 'NONE',  ( 0.000000000000000000, 0.000000000000000000, 1.000000000000000000 ) ) ;
#6138 = EDGE_CURVE ( 'NONE', #882, #9819, #4194, .T. ) ;
#6140 = ORIENTED_EDGE ( 'NONE', *, *, #6766, .T. ) ;
#6139 = EDGE_CURVE ( 'NONE', #8527, #10488, #1615, .T. ) ;
#6141 = ADVANCED_FACE ( 'NONE', ( #585 ), #15088, .T. ) ;
#6142 = PRODUCT_DEFINITION_SHAPE ( 'NONE', 'NONE',  #8102 ) ;
#6143 = DIRECTION ( 'NONE',  ( -0.000000000000000000, -0.000000000000000000, 1.000000000000000000 ) ) ;
#6144 = LINE ( 'NONE', #4070, #15543 ) ;
#6145 = VERTEX_POINT ( 'NONE', #4686 ) ;
#6146 = LINE ( 'NONE', #5024, #6289 ) ;
#6147 = CIRCLE ( 'NONE', #14117, 3.300000000000025135 ) ;
#6148 = CARTESIAN_POINT ( 'NONE',  ( -3.269999999998768114, 193.4898140233618449, 37.52989836422147363 ) ) ;
#6149 = FACE_OUTER_BOUND ( 'NONE', #15097, .T. ) ;
#6150 = CIRCLE ( 'NONE', #4244, 12.65000000000000036 ) ;
#6151 = CARTESIAN_POINT ( 'NONE',  ( 31.00000000000003553, 19.00000000000000000, 25.99999999999999645 ) ) ;
#6152 = DIRECTION ( 'NONE',  ( -0.000000000000000000, -1.000000000000000000, -0.000000000000000000 ) ) ;
#6153 = VERTEX_POINT ( 'NONE', #8484 ) ;
#6154 = CARTESIAN_POINT ( 'NONE',  ( 0.000000000000000000, 355.3192028797624857, -29.71049682360898814 ) ) ;
#6155 = B_SPLINE_SURFACE_WITH_KNOTS ( 'NONE', 1, 3, ( 
 ( #1433, #242, #9519, #5459, #326, #3069, #6827, #12086, #2899, #8135 ),
 ( #14577, #15940, #10539, #12265, #5548, #5378, #9427, #14757, #13557, #4364 ),
 ( #10799, #1787, #5288, #16039, #15773, #4185, #9596, #2805, #8041, #4020 ),
 ( #9258, #11919, #10625, #13302, #14672, #14497, #2719, #2980, #15856, #13384 ) ),
 .UNSPECIFIED., .F., .F., .F.,
 ( 2, 1, 1, 2 ),
 ( 4, 2, 2, 2, 4 ),
 ( -0.01000000000000000021, 0.000000000000000000, 1.000000000000000000, 1.010099999999999998 ),
 ( 0.000000000000000000, 0.2500000000000000000, 0.5000000000000000000, 0.7500000000000000000, 1.000000000000000000 ),
 .UNSPECIFIED. ) ;
#6156 = CARTESIAN_POINT ( 'NONE',  ( 39.09977993252485362, 344.7110430980827687, -6.736600000000000144 ) ) ;
#6157 = CARTESIAN_POINT ( 'NONE',  ( 31.00000000000001421, 10.00000000000000000, 25.99999999999999645 ) ) ;
#6158 = ORIENTED_EDGE ( 'NONE', *, *, #4887, .F. ) ;
#6159 = CIRCLE ( 'NONE', #14402, 10.00000000000000178 ) ;
#6160 = ADVANCED_FACE ( 'NONE', ( #7344 ), #1018, .T. ) ;
#6161 = CARTESIAN_POINT ( 'NONE',  ( 1.224999999999999867, -15.25000000000000000, -1.867586368699713770E-15 ) ) ;
#6162 = FACE_OUTER_BOUND ( 'NONE', #1473, .T. ) ;
#6163 = ORIENTED_EDGE ( 'NONE', *, *, #12151, .F. ) ;
#6164 = DIRECTION ( 'NONE',  ( 0.000000000000000000, 0.000000000000000000, -1.000000000000000000 ) ) ;
#6165 = PLANE ( 'NONE',  #247 ) ;
#6166 = CARTESIAN_POINT ( 'NONE',  ( -31.00000000000001776, 10.00000000000000000, 31.00000000000000000 ) ) ;
#6167 = VERTEX_POINT ( 'NONE', #9944 ) ;
#6168 = LINE ( 'NONE', #15620, #564 ) ;
#6169 = PLANE ( 'NONE',  #1580 ) ;
#6170 = CARTESIAN_POINT ( 'NONE',  ( -31.00000000000002132, 10.00000000000000000, -31.00000000000000000 ) ) ;
#6171 = ORIENTED_EDGE ( 'NONE', *, *, #6223, .F. ) ;
#6172 = LINE ( 'NONE', #6415, #2307 ) ;
#6173 = CIRCLE ( 'NONE', #11660, 4.999999999999997335 ) ;
#6174 = EDGE_CURVE ( 'NONE', #15212, #1142, #6470, .T. ) ;
#6175 = ITEM_DEFINED_TRANSFORMATION ( 'NONE', 'NONE', #6699,  #1488 ) ;
#6176 = DIRECTION ( 'NONE',  ( 0.000000000000000000, 0.000000000000000000, -1.000000000000000000 ) ) ;
#6177 = ORIENTED_EDGE ( 'NONE', *, *, #15524, .F. ) ;
#6178 = DIRECTION ( 'NONE',  ( 0.000000000000000000, 0.000000000000000000, 1.000000000000000000 ) ) ;
#6179 = CYLINDRICAL_SURFACE ( 'NONE', #1491, 3.299999999999997158 ) ;
#6180 = AXIS2_PLACEMENT_3D ( 'NONE', #9015, #10303, #12794 ) ;
#6181 = ORIENTED_EDGE ( 'NONE', *, *, #7467, .T. ) ;
#6182 = VECTOR ( 'NONE', #6855, 1000.000000000000000 ) ;
#6183 = CARTESIAN_POINT ( 'NONE',  ( 394.0000000000001137, 451.4647406485092915, -149.8062676851188257 ) ) ;
#6184 = CARTESIAN_POINT ( 'NONE',  ( 17.00000000000000711, 0.000000000000000000, -17.00000000000000355 ) ) ;
#6185 = VERTEX_POINT ( 'NONE', #838 ) ;
#6186 = FACE_OUTER_BOUND ( 'NONE', #13690, .T. ) ;
#6187 = ORIENTED_EDGE ( 'NONE', *, *, #7477, .F. ) ;
#6188 = VERTEX_POINT ( 'NONE', #12270 ) ;
#6189 = VERTEX_POINT ( 'NONE', #3330 ) ;
#6190 = VECTOR ( 'NONE', #4374, 1000.000000000000000 ) ;
#6191 = VECTOR ( 'NONE', #332, 1000.000000000000000 ) ;
#6192 = ORIENTED_EDGE ( 'NONE', *, *, #5607, .T. ) ;
#6193 = EDGE_LOOP ( 'NONE', ( #305, #8984, #5971, #15410 ) ) ;
#6194 = DIRECTION ( 'NONE',  ( 0.000000000000000000, 1.000000000000000000, 0.000000000000000000 ) ) ;
#6195 = LINE ( 'NONE', #10085, #15728 ) ;
#6196 = APPLICATION_CONTEXT ( 'automotive_design' ) ;
#6197 = CARTESIAN_POINT ( 'NONE',  ( -2.220446049250313081E-13, 135.5000000000000000, 3.000000000000000000 ) ) ;
#6198 = DIRECTION ( 'NONE',  ( 1.000000000000000000, 0.000000000000000000, 0.000000000000000000 ) ) ;
#6199 = LINE ( 'NONE', #5165, #5593 ) ;
#6200 = CIRCLE ( 'NONE', #5683, 15.25000000000000000 ) ;
#6201 = EDGE_CURVE ( 'NONE', #9177, #6935, #3249, .T. ) ;
#6202 = CARTESIAN_POINT ( 'NONE',  ( 54.99999999999999289, 515.4878487013597805, -734.2230258972047068 ) ) ;
#6203 = FACE_BOUND ( 'NONE', #6874, .T. ) ;
#6204 = ORIENTED_EDGE ( 'NONE', *, *, #1544, .F. ) ;
#6205 = CARTESIAN_POINT ( 'NONE',  ( -31.00000000000000000, 19.00000000000000000, 30.99999999999999289 ) ) ;
#6206 = CARTESIAN_POINT ( 'NONE',  ( 0.000000000000000000, 50.00000000000000000, 0.000000000000000000 ) ) ;
#6207 = VERTEX_POINT ( 'NONE', #8570 ) ;
#6208 = CARTESIAN_POINT ( 'NONE',  ( -37.00000000000000000, 68.00000000000000000, 23.00000000000000355 ) ) ;
#6210 = ORIENTED_EDGE ( 'NONE', *, *, #5156, .F. ) ;
#6209 = ORIENTED_EDGE ( 'NONE', *, *, #15086, .F. ) ;
#6211 = EDGE_CURVE ( 'NONE', #6345, #4991, #15264, .T. ) ;
#6212 = DIRECTION ( 'NONE',  ( 1.000000000000000000, 0.000000000000000000, 0.000000000000000000 ) ) ;
#6213 = EDGE_LOOP ( 'NONE', ( #8966, #9474, #4287, #3289 ) ) ;
#6214 = AXIS2_PLACEMENT_3D ( 'NONE', #14910, #7076, #5715 ) ;
#6215 = DIRECTION ( 'NONE',  ( 1.000000000000000000, 0.000000000000000000, 0.000000000000000000 ) ) ;
#6216 = LINE ( 'NONE', #7418, #15111 ) ;
#6217 = CARTESIAN_POINT ( 'NONE',  ( 17.00000000000000000, 380.0000000000000000, -65.00000000000000000 ) ) ;
#6218 = EDGE_LOOP ( 'NONE', ( #5157, #14670 ) ) ;
#6219 = UNCERTAINTY_MEASURE_WITH_UNIT (LENGTH_MEASURE( 1.000000000000000082E-05 ), #14018, 'distance_accuracy_value', 'NONE');
#6220 = FACE_OUTER_BOUND ( 'NONE', #6255, .T. ) ;
#6221 = FACE_OUTER_BOUND ( 'NONE', #5695, .T. ) ;
#6223 = EDGE_CURVE ( 'NONE', #13441, #10385, #3754, .T. ) ;
#6222 = ORIENTED_EDGE ( 'NONE', *, *, #2360, .T. ) ;
#6224 = DIRECTION ( 'NONE',  ( -0.000000000000000000, -1.000000000000000000, 0.000000000000000000 ) ) ;
#6225 = CARTESIAN_POINT ( 'NONE',  ( 0.1739760006947971005, 193.0429700394134613, 37.40680846401803450 ) ) ;
#6226 = CARTESIAN_POINT ( 'NONE',  ( 31.00000000000004263, 0.000000000000000000, -25.99999999999999645 ) ) ;
#6227 = CIRCLE ( 'NONE', #8983, 3.299999999999997158 ) ;
#6228 = DIRECTION ( 'NONE',  ( 4.868293667060507742E-17, -0.09950371902099772181, 0.9950371902099892640 ) ) ;
#6229 = LINE ( 'NONE', #1260, #12079 ) ;
#6230 = EDGE_LOOP ( 'NONE', ( #10277, #16629, #8332, #13551 ) ) ;
#6231 = EDGE_CURVE ( 'NONE', #16287, #3064, #1280, .T. ) ;
#6232 = EDGE_CURVE ( 'NONE', #2950, #11164, #14931, .T. ) ;
#6233 = PLANE ( 'NONE',  #4274 ) ;
#6234 = EDGE_CURVE ( 'NONE', #1137, #3021, #12526, .T. ) ;
#6235 = DIRECTION ( 'NONE',  ( 1.000000000000000000, 0.000000000000000000, -0.000000000000000000 ) ) ;
#6236 = DIRECTION ( 'NONE',  ( 0.000000000000000000, 0.000000000000000000, 1.000000000000000000 ) ) ;
#6237 = ORIENTED_EDGE ( 'NONE', *, *, #8673, .F. ) ;
#6238 = CIRCLE ( 'NONE', #9565, 0.9999999999999983347 ) ;
#6239 = CARTESIAN_POINT ( 'NONE',  ( 10.00000000000000000, 5.352861011586007481E-13, -75.00000000000599698 ) ) ;
#6240 = DIRECTION ( 'NONE',  ( 0.000000000000000000, 1.000000000000000000, 0.000000000000000000 ) ) ;
#6241 = EDGE_LOOP ( 'NONE', ( #6888, #12741, #5239, #16156 ) ) ;
#6242 = DIRECTION ( 'NONE',  ( 0.000000000000000000, 0.000000000000000000, -1.000000000000000000 ) ) ;
#6243 = CARTESIAN_POINT ( 'NONE',  ( -49.99999999999999289, 515.4878487013597805, -546.7230258972048205 ) ) ;
#6244 = ORIENTED_EDGE ( 'NONE', *, *, #3634, .T. ) ;
#6245 = PRESENTATION_STYLE_ASSIGNMENT (( #12798 ) ) ;
#6246 = CARTESIAN_POINT ( 'NONE',  ( 415.0210210471910841, 329.6061121441327941, 0.000000000000000000 ) ) ;
#6247 = DIRECTION ( 'NONE',  ( 0.000000000000000000, 1.000000000000000000, 0.000000000000000000 ) ) ;
#6248 = ORIENTED_EDGE ( 'NONE', *, *, #6032, .T. ) ;
#6249 = EDGE_CURVE ( 'NONE', #15569, #4190, #15275, .T. ) ;
#6250 = EDGE_CURVE ( 'NONE', #4652, #7581, #4579, .T. ) ;
#6251 = DIRECTION ( 'NONE',  ( -1.000000000000000000, 0.000000000000000000, 1.196361017915039732E-16 ) ) ;
#6252 = ADVANCED_FACE ( 'NONE', ( #13647, #7094 ), #15013, .F. ) ;
#6253 = AXIS2_PLACEMENT_3D ( 'NONE', #8931, #14169, #7620 ) ;
#6254 = CONTEXT_DEPENDENT_SHAPE_REPRESENTATION ( #10180, #16051 ) ;
#6255 = EDGE_LOOP ( 'NONE', ( #12063, #11659, #459, #12207 ) ) ;
#6256 = CYLINDRICAL_SURFACE ( 'NONE', #2245, 5.000000000000004441 ) ;
#6257 = CARTESIAN_POINT ( 'NONE',  ( 1.347066989204613998E-15, 0.000000000000000000, 22.00000000000000000 ) ) ;
#6258 = CARTESIAN_POINT ( 'NONE',  ( 1.224646799147351235E-16, 65.20000000000000284, -0.9999999999999988898 ) ) ;
#6259 = ORIENTED_EDGE ( 'NONE', *, *, #998, .T. ) ;
#6260 = CARTESIAN_POINT ( 'NONE',  ( -26.00000000000002842, 3.000000000000000000, -31.00000000000003197 ) ) ;
#6261 = DIRECTION ( 'NONE',  ( 1.000000000000000000, 0.000000000000000000, 0.000000000000000000 ) ) ;
#6262 = ORIENTED_EDGE ( 'NONE', *, *, #14550, .F. ) ;
#6263 = CARTESIAN_POINT ( 'NONE',  ( -46.99999999999988631, 549.5810598491746077, -531.8108303813202156 ) ) ;
#6264 = VERTEX_POINT ( 'NONE', #16300 ) ;
#6265 = ORIENTED_EDGE ( 'NONE', *, *, #16426, .F. ) ;
#6266 = CIRCLE ( 'NONE', #12056, 9.000000000000007105 ) ;
#6267 = LINE ( 'NONE', #2594, #12453 ) ;
#6268 = VERTEX_POINT ( 'NONE', #8656 ) ;
#6269 = EDGE_LOOP ( 'NONE', ( #16532, #15877, #14043, #8454 ) ) ;
#6270 = EDGE_LOOP ( 'NONE', ( #9001, #3257 ) ) ;
#6271 = CARTESIAN_POINT ( 'NONE',  ( 394.0000000000001137, 339.1725919290087745, -16.41886574335978821 ) ) ;
#6272 = CARTESIAN_POINT ( 'NONE',  ( -270.0000000000000000, 620.7506394335853201, -11.00000000000000000 ) ) ;
#6273 = AXIS2_PLACEMENT_3D ( 'NONE', #7186, #12443, #15100 ) ;
#6274 = DIRECTION ( 'NONE',  ( 6.092845550115373211E-18, 0.9950371902099904853, 0.09950371902098546772 ) ) ;
#6275 = CARTESIAN_POINT ( 'NONE',  ( 17.00000000000000000, 0.000000000000000000, -75.00000000000000000 ) ) ;
#6276 = CARTESIAN_POINT ( 'NONE',  ( -55.99999999999989342, 523.2161522479888163, -502.8936384967199729 ) ) ;
#6277 = EDGE_CURVE ( 'NONE', #3043, #12295, #1947, .T. ) ;
#6278 = CARTESIAN_POINT ( 'NONE',  ( 10.00000000000000000, 226.8713558223388134, -333.7582248962859808 ) ) ;
#6279 = LINE ( 'NONE', #13005, #8602 ) ;
#6280 = ORIENTED_EDGE ( 'NONE', *, *, #15293, .F. ) ;
#6281 = DIRECTION ( 'NONE',  ( 0.000000000000000000, 0.000000000000000000, 1.000000000000000000 ) ) ;
#6282 = LINE ( 'NONE', #3813, #13796 ) ;
#6283 = VERTEX_POINT ( 'NONE', #4447 ) ;
#6284 = EDGE_CURVE ( 'NONE', #16344, #11779, #6057, .T. ) ;
#6285 = DIRECTION ( 'NONE',  ( 0.000000000000000000, 0.000000000000000000, -1.000000000000000000 ) ) ;
#6287 = ORIENTED_EDGE ( 'NONE', *, *, #3922, .T. ) ;
#6286 = ORIENTED_EDGE ( 'NONE', *, *, #8046, .T. ) ;
#6288 = CARTESIAN_POINT ( 'NONE',  ( 75.00000000000000000, 355.3192028797624857, -29.71049682360898814 ) ) ;
#6289 = VECTOR ( 'NONE', #10110, 1000.000000000000000 ) ;
#6290 = ORIENTED_EDGE ( 'NONE', *, *, #4267, .T. ) ;
#6291 = DIRECTION ( 'NONE',  ( 0.000000000000000000, 0.000000000000000000, 1.000000000000000000 ) ) ;
#6292 = EDGE_CURVE ( 'NONE', #9971, #7606, #14201, .T. ) ;
#6293 = VECTOR ( 'NONE', #3563, 1000.000000000000000 ) ;
#6294 = DIRECTION ( 'NONE',  ( 0.000000000000000000, 0.000000000000000000, -1.000000000000000000 ) ) ;
#6295 = CARTESIAN_POINT ( 'NONE',  ( 10.00000000000000000, 372.8685141053778693, -83.18019484660869978 ) ) ;
#6296 = ORIENTED_EDGE ( 'NONE', *, *, #4256, .F. ) ;
#6297 = CARTESIAN_POINT ( 'NONE',  ( 1.223489862255693833E-15, 380.0000000000000000, -75.00000000000000000 ) ) ;
#6298 = ADVANCED_FACE ( 'NONE', ( #11788 ), #10190, .T. ) ;
#6299 = CIRCLE ( 'NONE', #1655, 3.300000000000025135 ) ;
#6300 = ORIENTED_EDGE ( 'NONE', *, *, #16315, .F. ) ;
#6301 = CARTESIAN_POINT ( 'NONE',  ( 415.0210210471910841, 329.6061121441327941, -6.736600000000000144 ) ) ;
#6302 = CIRCLE ( 'NONE', #11488, 13.29999999999999893 ) ;
#6303 = CARTESIAN_POINT ( 'NONE',  ( 0.000000000000000000, 0.000000000000000000, 0.000000000000000000 ) ) ;
#6304 = CARTESIAN_POINT ( 'NONE',  ( 2.625000000000000000, 14.59999999999999964, 0.000000000000000000 ) ) ;
#6305 = DIRECTION ( 'NONE',  ( 0.000000000000000000, -0.7208880098054721852, 0.6930515690182841304 ) ) ;
#6306 = DIRECTION ( 'NONE',  ( -0.000000000000000000, -0.000000000000000000, 1.000000000000000000 ) ) ;
#6307 = EDGE_LOOP ( 'NONE', ( #8253, #7647, #451, #2596 ) ) ;
#6308 = DIRECTION ( 'NONE',  ( 1.000000000000000000, 0.000000000000000000, -0.000000000000000000 ) ) ;
#6309 = VECTOR ( 'NONE', #1269, 1000.000000000000000 ) ;
#6310 = DIRECTION ( 'NONE',  ( 1.000000000000000000, -0.000000000000000000, -0.000000000000000000 ) ) ;
#6311 = ADVANCED_FACE ( 'NONE', ( #2769 ), #3892, .T. ) ;
#6312 = EDGE_CURVE ( 'NONE', #5074, #3738, #11698, .T. ) ;
#6313 =( REPRESENTATION_RELATIONSHIP ('NONE','NONE', #15277, #135 ) REPRESENTATION_RELATIONSHIP_WITH_TRANSFORMATION ( #12546 )SHAPE_REPRESENTATION_RELATIONSHIP( ) );
#6314 = DIRECTION ( 'NONE',  ( 0.9999937692730440641, 0.003530072958125829961, 0.000000000000000000 ) ) ;
#6315 = ORIENTED_EDGE ( 'NONE', *, *, #13473, .T. ) ;
#6316 = DIRECTION ( 'NONE',  ( 0.000000000000000000, 1.000000000000000000, 0.000000000000000000 ) ) ;
#6317 = ADVANCED_FACE ( 'NONE', ( #6221 ), #2198, .F. ) ;
#6318 = DIRECTION ( 'NONE',  ( 6.123031769111888756E-17, 0.000000000000000000, 1.000000000000000000 ) ) ;
#6319 = VERTEX_POINT ( 'NONE', #8817 ) ;
#6320 = DIRECTION ( 'NONE',  ( 1.000000000000000000, 0.000000000000000000, -0.000000000000000000 ) ) ;
#6321 = CARTESIAN_POINT ( 'NONE',  ( 1.286622718088548112E-12, 258.8496290447203023, 286.9685381829918924 ) ) ;
#6322 = DIRECTION ( 'NONE',  ( 0.000000000000000000, 0.000000000000000000, -1.000000000000000000 ) ) ;
#6323 = ORIENTED_EDGE ( 'NONE', *, *, #3297, .F. ) ;
#6324 = CIRCLE ( 'NONE', #9917, 0.7366000000000004766 ) ;
#6325 = DIRECTION ( 'NONE',  ( 0.000000000000000000, 0.000000000000000000, 1.000000000000000000 ) ) ;
#6326 = CARTESIAN_POINT ( 'NONE',  ( 75.00000000000000000, 0.000000000000000000, 0.000000000000000000 ) ) ;
#6327 = ORIENTED_EDGE ( 'NONE', *, *, #2445, .T. ) ;
#6328 = DIRECTION ( 'NONE',  ( 0.000000000000000000, 0.000000000000000000, 1.000000000000000000 ) ) ;
#6329 = AXIS2_PLACEMENT_3D ( 'NONE', #10295, #16715, #10202 ) ;
#6330 = ADVANCED_FACE ( 'NONE', ( #3582 ), #2608, .F. ) ;
#6331 = AXIS2_PLACEMENT_3D ( 'NONE', #16491, #713, #9816 ) ;
#6332 = VERTEX_POINT ( 'NONE', #11470 ) ;
#6333 = CARTESIAN_POINT ( 'NONE',  ( -37.00000000000000000, 0.000000000000000000, 23.00000000000000355 ) ) ;
#6334 = ADVANCED_FACE ( 'NONE', ( #6717 ), #123, .F. ) ;
#6335 = CARTESIAN_POINT ( 'NONE',  ( 39.41161623800082481, 323.9612906317821057, -10.00000000000000000 ) ) ;
#6336 = ADVANCED_FACE ( 'NONE', ( #5348, #5429 ), #1492, .T. ) ;
#6337 = EDGE_CURVE ( 'NONE', #544, #14215, #3220, .T. ) ;
#6338 = VECTOR ( 'NONE', #5111, 1000.000000000000000 ) ;
#6339 = PLANE ( 'NONE',  #12360 ) ;
#6340 = ORIENTED_EDGE ( 'NONE', *, *, #13422, .T. ) ;
#6341 = CARTESIAN_POINT ( 'NONE',  ( 0.000000000000000000, 0.000000000000000000, 0.000000000000000000 ) ) ;
#6342 = EDGE_CURVE ( 'NONE', #2707, #8178, #4145, .T. ) ;
#6343 =( GEOMETRIC_REPRESENTATION_CONTEXT ( 3 ) GLOBAL_UNCERTAINTY_ASSIGNED_CONTEXT ( ( #6055 ) ) GLOBAL_UNIT_ASSIGNED_CONTEXT ( ( #1412, #5444, #16102 ) ) REPRESENTATION_CONTEXT ( 'NONE', 'WORKASPACE' ) );
#6344 = FACE_OUTER_BOUND ( 'NONE', #1454, .T. ) ;
#6345 = VERTEX_POINT ( 'NONE', #5245 ) ;
#6346 = CARTESIAN_POINT ( 'NONE',  ( 46.99999999999988631, 473.6663340069157471, -526.8058340126048051 ) ) ;
#6347 = EDGE_LOOP ( 'NONE', ( #3710, #5937, #13572, #2880 ) ) ;
#6348 = VERTEX_POINT ( 'NONE', #2687 ) ;
#6349 = VECTOR ( 'NONE', #8698, 1000.000000000000000 ) ;
#6350 = DIRECTION ( 'NONE',  ( 0.000000000000000000, 0.000000000000000000, -1.000000000000000000 ) ) ;
#6351 = ORIENTED_EDGE ( 'NONE', *, *, #10552, .T. ) ;
#6352 = PRODUCT_DEFINITION_CONTEXT ( 'detailed design', #1071, 'design' ) ;
#6353 = VECTOR ( 'NONE', #9770, 1000.000000000000000 ) ;
#6354 = AXIS2_PLACEMENT_3D ( 'NONE', #1806, #13658, #16221 ) ;
#6355 = VERTEX_POINT ( 'NONE', #11393 ) ;
#6356 = ORIENTED_EDGE ( 'NONE', *, *, #16337, .T. ) ;
#6357 = DIRECTION ( 'NONE',  ( -1.000000000000000000, -0.000000000000000000, -0.000000000000000000 ) ) ;
#6358 = FACE_OUTER_BOUND ( 'NONE', #2079, .T. ) ;
#6359 = ORIENTED_EDGE ( 'NONE', *, *, #10182, .T. ) ;
#6360 = DIRECTION ( 'NONE',  ( 0.000000000000000000, 0.000000000000000000, -1.000000000000000000 ) ) ;
#6361 = EDGE_CURVE ( 'NONE', #12007, #13963, #6144, .T. ) ;
#6362 = CONICAL_SURFACE ( 'NONE', #16534, 13.89560290347679938, 1.567266246505109928 ) ;
#6363 = CARTESIAN_POINT ( 'NONE',  ( 5.941205806953520074, 0.000000000000000000, 0.000000000000000000 ) ) ;
#6364 = TOROIDAL_SURFACE ( 'NONE', #9409, 4.695405383895982609, 9.000000000000000000 ) ;
#6365 = ORIENTED_EDGE ( 'NONE', *, *, #11263, .F. ) ;
#6366 = CARTESIAN_POINT ( 'NONE',  ( 0.000000000000000000, 339.1725919290087745, -10.68226574335978718 ) ) ;
#6367 = DIRECTION ( 'NONE',  ( 0.000000000000000000, -1.000000000000000000, 0.000000000000000000 ) ) ;
#6368 = VERTEX_POINT ( 'NONE', #10502 ) ;
#6369 = DIRECTION ( 'NONE',  ( 0.000000000000000000, 0.000000000000000000, -1.000000000000000000 ) ) ;
#6370 = EDGE_LOOP ( 'NONE', ( #8342, #307 ) ) ;
#6371 = AXIS2_PLACEMENT_3D ( 'NONE', #14123, #2343, #11202 ) ;
#6372 = DIRECTION ( 'NONE',  ( -1.000000000000000000, -0.000000000000000000, -0.000000000000000000 ) ) ;
#6373 = ORIENTED_EDGE ( 'NONE', *, *, #11255, .F. ) ;
#6374 = ADVANCED_FACE ( 'NONE', ( #15740 ), #11431, .F. ) ;
#6375 = AXIS2_PLACEMENT_3D ( 'NONE', #5089, #13175, #3737 ) ;
#6376 = ORIENTED_EDGE ( 'NONE', *, *, #12551, .F. ) ;
#6377 = AXIS2_PLACEMENT_3D ( 'NONE', #15242, #1925, #7406 ) ;
#6378 = VECTOR ( 'NONE', #8812, 1000.000000000000000 ) ;
#6379 = CARTESIAN_POINT ( 'NONE',  ( 7.000000000000001776, 380.0000000000000000, -75.00000000000000000 ) ) ;
#6380 = DIRECTION ( 'NONE',  ( -0.000000000000000000, 0.000000000000000000, -1.000000000000000000 ) ) ;
#6381 = EDGE_LOOP ( 'NONE', ( #6710, #12604 ) ) ;
#6382 = CARTESIAN_POINT ( 'NONE',  ( 56.73000000000001108, 192.7170024689953891, 37.20452120302230981 ) ) ;
#6383 = DIRECTION ( 'NONE',  ( 0.000000000000000000, 1.000000000000000000, 0.000000000000000000 ) ) ;
#6384 = AXIS2_PLACEMENT_3D ( 'NONE', #11347, #7555, #2585 ) ;
#6385 = CARTESIAN_POINT ( 'NONE',  ( -54.99999999999999289, 515.4878487013597805, -546.7230258972048205 ) ) ;
#6386 = CARTESIAN_POINT ( 'NONE',  ( 0.5524412557582074612, 192.7747313313365112, 37.26585803622744919 ) ) ;
#6387 = CARTESIAN_POINT ( 'NONE',  ( 55.99999999999989342, 549.5810598491746077, -518.1154249974242703 ) ) ;
#6388 = VECTOR ( 'NONE', #13263, 1000.000000000000000 ) ;
#6389 = FACE_OUTER_BOUND ( 'NONE', #4519, .T. ) ;
#6390 = AXIS2_PLACEMENT_3D ( 'NONE', #9500, #5710, #141 ) ;
#6391 = DIRECTION ( 'NONE',  ( -7.213771534993946619E-17, -0.09950371902098976984, -0.9950371902099900412 ) ) ;
#6393 = ORIENTED_EDGE ( 'NONE', *, *, #4488, .F. ) ;
#6392 = ORIENTED_EDGE ( 'NONE', *, *, #6361, .F. ) ;
#6394 = LINE ( 'NONE', #9079, #8393 ) ;
#6395 = EDGE_CURVE ( 'NONE', #9705, #6745, #10592, .T. ) ;
#6396 = VECTOR ( 'NONE', #15002, 1000.000000000000000 ) ;
#6397 = VECTOR ( 'NONE', #13047, 1000.000000000000114 ) ;
#6398 = CARTESIAN_POINT ( 'NONE',  ( 54.99999999999999289, 515.4878487013597805, -734.2230258972047068 ) ) ;
#6399 = DIRECTION ( 'NONE',  ( 0.000000000000000000, 0.000000000000000000, 1.000000000000000000 ) ) ;
#6400 = AXIS2_PLACEMENT_3D ( 'NONE', #5588, #2843, #1727 ) ;
#6401 = VERTEX_POINT ( 'NONE', #921 ) ;
#6402 = DIRECTION ( 'NONE',  ( -1.000000000000000000, 0.000000000000000000, -0.000000000000000000 ) ) ;
#6403 = DIRECTION ( 'NONE',  ( 0.000000000000000000, 0.000000000000000000, 1.000000000000000000 ) ) ;
#6404 = ORIENTED_EDGE ( 'NONE', *, *, #9934, .T. ) ;
#6405 = CARTESIAN_POINT ( 'NONE',  ( 6.183064636039277557E-13, 183.8715257629572193, -18.38715257629583633 ) ) ;
#6406 = TOROIDAL_SURFACE ( 'NONE', #12203, 4.695405383895982609, 9.000000000000000000 ) ;
#6407 = DIRECTION ( 'NONE',  ( 0.000000000000000000, 0.000000000000000000, -1.000000000000000000 ) ) ;
#6408 = LINE ( 'NONE', #5210, #10316 ) ;
#6409 = ORIENTED_EDGE ( 'NONE', *, *, #10007, .F. ) ;
#6410 = EDGE_CURVE ( 'NONE', #12590, #14388, #16898, .T. ) ;
#6411 = DIRECTION ( 'NONE',  ( 0.000000000000000000, 0.000000000000000000, 1.000000000000000000 ) ) ;
#6412 = LINE ( 'NONE', #6680, #1866 ) ;
#6413 = CARTESIAN_POINT ( 'NONE',  ( 0.000000000000000000, 2.755455298081544778E-15, -22.50000000000000000 ) ) ;
#6414 = ORIENTED_EDGE ( 'NONE', *, *, #11799, .F. ) ;
#6415 = CARTESIAN_POINT ( 'NONE',  ( 21.00000000000000000, 19.00000000000000000, 31.00000000000006395 ) ) ;
#6416 = ORIENTED_EDGE ( 'NONE', *, *, #15759, .T. ) ;
#6417 = APPLICATION_CONTEXT ( 'automotive_design' ) ;
#6418 = EDGE_CURVE ( 'NONE', #4822, #4318, #7514, .T. ) ;
#6419 = AXIS2_PLACEMENT_3D ( 'NONE', #11068, #7183, #1803 ) ;
#6420 = FACE_OUTER_BOUND ( 'NONE', #15797, .T. ) ;
#6421 = ORIENTED_EDGE ( 'NONE', *, *, #10334, .T. ) ;
#6422 = LINE ( 'NONE', #4974, #10759 ) ;
#6423 = CARTESIAN_POINT ( 'NONE',  ( -20.99999999999999645, 19.00000000000000000, -35.00000000000000711 ) ) ;
#6424 = CARTESIAN_POINT ( 'NONE',  ( 21.99999999999998224, 6.000000000000000000, -35.99999999999999289 ) ) ;
#6425 = EDGE_LOOP ( 'NONE', ( #9219, #6177, #420, #11819 ) ) ;
#6426 = DIRECTION ( 'NONE',  ( 0.000000000000000000, 0.000000000000000000, -1.000000000000000000 ) ) ;
#6427 = DIRECTION ( 'NONE',  ( 1.000000000000000000, 0.000000000000000000, -0.000000000000000000 ) ) ;
#6428 = ORIENTED_EDGE ( 'NONE', *, *, #6976, .F. ) ;
#6429 = EDGE_CURVE ( 'NONE', #10488, #6355, #8363, .T. ) ;
#6430 = VECTOR ( 'NONE', #7251, 1000.000000000000000 ) ;
#6431 = DIRECTION ( 'NONE',  ( 0.000000000000000000, 0.000000000000000000, 1.000000000000000000 ) ) ;
#6432 = ORIENTED_EDGE ( 'NONE', *, *, #1710, .F. ) ;
#6433 = EDGE_LOOP ( 'NONE', ( #3638, #7524 ) ) ;
#6434 = DIRECTION ( 'NONE',  ( 0.000000000000000000, 0.000000000000000000, 1.000000000000000000 ) ) ;
#6435 = ORIENTED_EDGE ( 'NONE', *, *, #1939, .F. ) ;
#6436 = EDGE_CURVE ( 'NONE', #5130, #10548, #6973, .T. ) ;
#6437 = EDGE_CURVE ( 'NONE', #15562, #2788, #12228, .T. ) ;
#6438 = EDGE_CURVE ( 'NONE', #7594, #9955, #16085, .T. ) ;
#6439 = EDGE_CURVE ( 'NONE', #4506, #6188, #16166, .T. ) ;
#6440 = ORIENTED_EDGE ( 'NONE', *, *, #5836, .F. ) ;
#6441 = CIRCLE ( 'NONE', #4286, 4.999999999999997335 ) ;
#6442 = ORIENTED_EDGE ( 'NONE', *, *, #3271, .F. ) ;
#6443 = VECTOR ( 'NONE', #2435, 1000.000000000000000 ) ;
#6444 = CARTESIAN_POINT ( 'NONE',  ( 10.00000000000000000, 381.0487089519832011, -80.00000000000332534 ) ) ;
#6445 = DIRECTION ( 'NONE',  ( -0.000000000000000000, 0.000000000000000000, 1.000000000000000000 ) ) ;
#6446 = ORIENTED_EDGE ( 'NONE', *, *, #6660, .F. ) ;
#6447 = CARTESIAN_POINT ( 'NONE',  ( 39.99999999999999289, 8.000000000000000000, 18.99999999999999645 ) ) ;
#6448 = CARTESIAN_POINT ( 'NONE',  ( 449.9999999999998295, 135.5000000000000000, 0.000000000000000000 ) ) ;
#6449 = FACE_OUTER_BOUND ( 'NONE', #9039, .T. ) ;
#6450 = EDGE_LOOP ( 'NONE', ( #9272, #5495 ) ) ;
#6451 = CARTESIAN_POINT ( 'NONE',  ( 0.6999999999999999556, -18.50000000000000000, -2.265596578422603396E-15 ) ) ;
#6452 = CARTESIAN_POINT ( 'NONE',  ( 394.0000000000001137, 451.4647406485092915, -149.8062676851188257 ) ) ;
#6453 = ADVANCED_BREP_SHAPE_REPRESENTATION ( '', ( #3006, #1488 ), #13292 ) ;
#6454 = ORIENTED_EDGE ( 'NONE', *, *, #7924, .T. ) ;
#6455 = AXIS2_PLACEMENT_3D ( 'NONE', #10050, #8680, #7365 ) ;
#6456 = CIRCLE ( 'NONE', #10319, 13.69540538389601991 ) ;
#6457 = CARTESIAN_POINT ( 'NONE',  ( -39.99999999999999289, 11.00000000000000000, 25.99999999999999645 ) ) ;
#6458 = ORIENTED_EDGE ( 'NONE', *, *, #3845, .F. ) ;
#6459 = EDGE_CURVE ( 'NONE', #14529, #3296, #15009, .T. ) ;
#6460 = EDGE_CURVE ( 'NONE', #3093, #976, #4312, .T. ) ;
#6461 = FACE_OUTER_BOUND ( 'NONE', #864, .T. ) ;
#6462 = EDGE_CURVE ( 'NONE', #10795, #7998, #5938, .T. ) ;
#6463 = EDGE_LOOP ( 'NONE', ( #11160, #576, #12876, #14382 ) ) ;
#6464 = ORIENTED_EDGE ( 'NONE', *, *, #2291, .F. ) ;
#6465 = SURFACE_STYLE_FILL_AREA ( #3662 ) ;
#6466 = DIRECTION ( 'NONE',  ( -0.000000000000000000, -1.000000000000000000, 0.000000000000000000 ) ) ;
#6467 = DIRECTION ( 'NONE',  ( 1.000000000000000000, -0.000000000000000000, 0.000000000000000000 ) ) ;
#6468 = CIRCLE ( 'NONE', #10066, 84.99999999999997158 ) ;
#6469 = ORIENTED_EDGE ( 'NONE', *, *, #259, .T. ) ;
#6470 = CIRCLE ( 'NONE', #7851, 17.85000000000000142 ) ;
#6471 = CARTESIAN_POINT ( 'NONE',  ( 0.000000000000000000, 309.2289037985890445, -146.8198051533984199 ) ) ;
#6472 = FACE_OUTER_BOUND ( 'NONE', #5480, .T. ) ;
#6473 = DIRECTION ( 'NONE',  ( 1.000000000000000000, 0.000000000000000000, 0.000000000000000000 ) ) ;
#6474 = EDGE_CURVE ( 'NONE', #6725, #14628, #2379, .T. ) ;
#6475 = FACE_BOUND ( 'NONE', #3486, .T. ) ;
#6476 = LINE ( 'NONE', #6226, #11037 ) ;
#6477 = DIRECTION ( 'NONE',  ( -1.000000000000000000, 0.000000000000000000, -0.000000000000000000 ) ) ;
#6478 = CARTESIAN_POINT ( 'NONE',  ( 21.99999999999998224, 10.00000000000000000, -32.99999999999999289 ) ) ;
#6480 = EDGE_LOOP ( 'NONE', ( #9458, #8091, #14807, #10373 ) ) ;
#6479 = ORIENTED_EDGE ( 'NONE', *, *, #13215, .F. ) ;
#6481 = AXIS2_PLACEMENT_3D ( 'NONE', #6205, #16612, #6281 ) ;
#6482 = LINE ( 'NONE', #16884, #7531 ) ;
#6483 = AXIS2_PLACEMENT_3D ( 'NONE', #1469, #2490, #7897 ) ;
#6484 = FACE_OUTER_BOUND ( 'NONE', #988, .T. ) ;
#6485 = CARTESIAN_POINT ( 'NONE',  ( 46.99999999999988631, 523.2161522479893847, -590.5524132976893270 ) ) ;
#6486 = DIRECTION ( 'NONE',  ( -0.000000000000000000, -1.000000000000000000, -0.000000000000000000 ) ) ;
#6487 = EDGE_LOOP ( 'NONE', ( #8920, #12522, #13357, #1174 ) ) ;
#6488 = DIRECTION ( 'NONE',  ( -1.000000000000000000, 0.000000000000000000, 0.000000000000000000 ) ) ;
#6489 = EDGE_CURVE ( 'NONE', #4994, #9380, #8136, .T. ) ;
#6490 = CARTESIAN_POINT ( 'NONE',  ( -55.99999999999989342, 493.2350855268086320, -512.8755148539809170 ) ) ;
#6491 = ORIENTED_EDGE ( 'NONE', *, *, #2149, .F. ) ;
#6492 = CARTESIAN_POINT ( 'NONE',  ( 0.000000000000000000, 411.2412070270587492, -605.3473189749742005 ) ) ;
#6493 = EDGE_CURVE ( 'NONE', #3466, #10713, #2942, .T. ) ;
#6494 = CARTESIAN_POINT ( 'NONE',  ( 394.0000000000001137, 339.3157724647196005, -110.6822657433597925 ) ) ;
#6495 = CARTESIAN_POINT ( 'NONE',  ( -36.00000000000000711, 10.00000000000000000, -18.00000000000000355 ) ) ;
#6496 = CARTESIAN_POINT ( 'NONE',  ( 31.00000000000002842, 0.000000000000000000, 23.00000000000001066 ) ) ;
#6497 = FACE_OUTER_BOUND ( 'NONE', #2726, .T. ) ;
#6498 = CARTESIAN_POINT ( 'NONE',  ( 10.00000000000000000, 309.2289037985885898, -86.48019484660916589 ) ) ;
#6499 = ORIENTED_EDGE ( 'NONE', *, *, #16397, .F. ) ;
#6500 = DIRECTION ( 'NONE',  ( 0.000000000000000000, 0.000000000000000000, -1.000000000000000000 ) ) ;
#6501 = ITEM_DEFINED_TRANSFORMATION ( 'NONE', 'NONE', #8628,  #9434 ) ;
#6502 = VECTOR ( 'NONE', #13980, 1000.000000000000000 ) ;
#6503 = SHAPE_REPRESENTATION_RELATIONSHIP ( 'NONE' , 'NONE' ,  #11211, #2183 ) ;
#6504 = CIRCLE ( 'NONE', #13941, 4.999999999999997335 ) ;
#6505 = CYLINDRICAL_SURFACE ( 'NONE', #9942, 3.299999999999997158 ) ;
#6506 = VERTEX_POINT ( 'NONE', #3037 ) ;
#6507 = EDGE_CURVE ( 'NONE', #13450, #16590, #8667, .T. ) ;
#6508 = DIRECTION ( 'NONE',  ( 1.000000000000000000, 0.000000000000000000, 0.000000000000000000 ) ) ;
#6509 = CARTESIAN_POINT ( 'NONE',  ( -26.00000000000002132, 0.000000000000000000, 40.00000000000000711 ) ) ;
#6510 = DIRECTION ( 'NONE',  ( 0.000000000000000000, -1.000000000000000000, 0.000000000000000000 ) ) ;
#6511 = ORIENTED_EDGE ( 'NONE', *, *, #16716, .F. ) ;
#6512 = DIRECTION ( 'NONE',  ( 0.000000000000000000, 0.000000000000000000, -1.000000000000000000 ) ) ;
#6513 = DIRECTION ( 'NONE',  ( 0.000000000000000000, 0.000000000000000000, -1.000000000000000000 ) ) ;
#6514 = DIRECTION ( 'NONE',  ( -1.000000000000000000, -0.000000000000000000, -0.000000000000000000 ) ) ;
#6515 = ORIENTED_EDGE ( 'NONE', *, *, #6232, .T. ) ;
#6516 = EDGE_CURVE ( 'NONE', #4443, #3814, #12238, .T. ) ;
#6517 = VECTOR ( 'NONE', #11417, 1000.000000000000000 ) ;
#6518 = DIRECTION ( 'NONE',  ( -1.000000000000000000, 0.000000000000000000, 0.000000000000000000 ) ) ;
#6519 = ORIENTED_EDGE ( 'NONE', *, *, #15459, .T. ) ;
#6520 = EDGE_LOOP ( 'NONE', ( #16096, #11270, #15534, #2463 ) ) ;
#6521 = FACE_OUTER_BOUND ( 'NONE', #5119, .T. ) ;
#6522 = ORIENTED_EDGE ( 'NONE', *, *, #13839, .T. ) ;
#6523 = DIRECTION ( 'NONE',  ( -1.387778780781445676E-17, 0.000000000000000000, -1.000000000000000222 ) ) ;
#6524 = ORIENTED_EDGE ( 'NONE', *, *, #3726, .T. ) ;
#6525 = EDGE_LOOP ( 'NONE', ( #10883, #1036, #14709, #8103 ) ) ;
#6526 = ADVANCED_FACE ( 'NONE', ( #10757 ), #13351, .F. ) ;
#6527 = CIRCLE ( 'NONE', #15331, 13.69540538389601991 ) ;
#6528 = EDGE_CURVE ( 'NONE', #4334, #9087, #1578, .T. ) ;
#6529 = FACE_OUTER_BOUND ( 'NONE', #7165, .T. ) ;
#6530 = CARTESIAN_POINT ( 'NONE',  ( 3.850000000000000089, 0.000000000000000000, 0.000000000000000000 ) ) ;
#6531 = EDGE_LOOP ( 'NONE', ( #10830, #9968, #7733, #16713, #887 ) ) ;
#6532 = CARTESIAN_POINT ( 'NONE',  ( 5.569974746830579804, 0.000000000000000000, 0.000000000000000000 ) ) ;
#6533 = EDGE_CURVE ( 'NONE', #4318, #12218, #13091, .T. ) ;
#6534 = CARTESIAN_POINT ( 'NONE',  ( 40.00000000000003553, 3.000000000000000000, 26.00000000000000355 ) ) ;
#6535 = EDGE_CURVE ( 'NONE', #14834, #3191, #4495, .T. ) ;
#6536 = ADVANCED_FACE ( 'NONE', ( #13520 ), #5691, .T. ) ;
#6537 = FACE_OUTER_BOUND ( 'NONE', #7843, .T. ) ;
#6538 = EDGE_LOOP ( 'NONE', ( #13448, #1534, #15758, #13758 ) ) ;
#6539 = DIRECTION ( 'NONE',  ( -0.000000000000000000, -1.000000000000000000, -0.000000000000000000 ) ) ;
#6540 = CARTESIAN_POINT ( 'NONE',  ( -46.99999999999988631, 523.2161522479893847, -590.5524132976893270 ) ) ;
#6541 = VERTEX_POINT ( 'NONE', #6880 ) ;
#6542 = DIRECTION ( 'NONE',  ( -1.104713198929451483E-16, -0.09950371902099953980, -0.9950371902099890420 ) ) ;
#6543 = ORIENTED_EDGE ( 'NONE', *, *, #4969, .F. ) ;
#6544 = PLANE ( 'NONE',  #2352 ) ;
#6545 = ORIENTED_EDGE ( 'NONE', *, *, #10576, .F. ) ;
#6546 = CIRCLE ( 'NONE', #2450, 13.69540538389601991 ) ;
#6547 = ORIENTED_EDGE ( 'NONE', *, *, #10665, .F. ) ;
#6548 = ADVANCED_FACE ( 'NONE', ( #12139 ), #2108, .T. ) ;
#6549 = CARTESIAN_POINT ( 'NONE',  ( 22.99999999999998224, 6.000000000000000000, -31.99999999999998579 ) ) ;
#6550 = CARTESIAN_POINT ( 'NONE',  ( -8.881784197001250351E-16, 17.85000000000000142, 0.000000000000000000 ) ) ;
#6551 = ORIENTED_EDGE ( 'NONE', *, *, #8705, .F. ) ;
#6552 = LINE ( 'NONE', #144, #3355 ) ;
#6553 = PRODUCT_DEFINITION_SHAPE ( 'NONE', 'NONE',  #14937 ) ;
#6554 = DIRECTION ( 'NONE',  ( -0.000000000000000000, 0.000000000000000000, -1.000000000000000000 ) ) ;
#6555 = EDGE_CURVE ( 'NONE', #777, #11379, #15048, .T. ) ;
#6556 = EDGE_CURVE ( 'NONE', #1693, #4232, #877, .T. ) ;
#6557 = EDGE_CURVE ( 'NONE', #10409, #3786, #12814, .T. ) ;
#6558 = CARTESIAN_POINT ( 'NONE',  ( 1.223489862255693833E-15, 380.0000000000000000, -75.00000000000000000 ) ) ;
#6559 = EDGE_CURVE ( 'NONE', #7606, #12146, #2326, .T. ) ;
#6560 = DIRECTION ( 'NONE',  ( 0.000000000000000000, -7.137148015447440312E-15, 1.000000000000000000 ) ) ;
#6561 = CARTESIAN_POINT ( 'NONE',  ( -0.9999999999999991118, 0.000000000000000000, 22.50000000000000000 ) ) ;
#6562 = AXIS2_PLACEMENT_3D ( 'NONE', #1014, #7771, #4945 ) ;
#6563 = CIRCLE ( 'NONE', #8235, 17.52499999999999858 ) ;
#6564 = DIRECTION ( 'NONE',  ( -1.000000000000000000, -0.000000000000000000, -0.000000000000000000 ) ) ;
#6565 = CARTESIAN_POINT ( 'NONE',  ( 55.99999999999989342, 473.6663340069157471, -531.5012393965008641 ) ) ;
#6567 = ORIENTED_EDGE ( 'NONE', *, *, #6460, .F. ) ;
#6566 = ORIENTED_EDGE ( 'NONE', *, *, #4402, .F. ) ;
#6568 = FACE_OUTER_BOUND ( 'NONE', #8532, .T. ) ;
#6569 = CARTESIAN_POINT ( 'NONE',  ( 449.9999999999998295, 135.5000000000000000, 0.000000000000000000 ) ) ;
#6570 = CARTESIAN_POINT ( 'NONE',  ( -33.00000000000000000, 8.000000000000000000, -22.00000000000000355 ) ) ;
#6571 = DIRECTION ( 'NONE',  ( -1.156482317317881191E-15, 0.000000000000000000, -1.000000000000000000 ) ) ;
#6572 = AXIS2_PLACEMENT_3D ( 'NONE', #6627, #11888, #131 ) ;
#6573 = ORIENTED_EDGE ( 'NONE', *, *, #1266, .F. ) ;
#6574 = AXIS2_PLACEMENT_3D ( 'NONE', #7407, #7488, #1062 ) ;
#6575 = DIRECTION ( 'NONE',  ( -1.000000000000000000, -0.000000000000000000, 0.000000000000000000 ) ) ;
#6576 = FACE_OUTER_BOUND ( 'NONE', #8086, .T. ) ;
#6577 = VERTEX_POINT ( 'NONE', #3372 ) ;
#6578 = DIRECTION ( 'NONE',  ( 0.000000000000000000, -1.000000000000000000, -0.000000000000000000 ) ) ;
#6579 = EDGE_CURVE ( 'NONE', #1698, #14192, #8613, .T. ) ;
#6580 = FACE_OUTER_BOUND ( 'NONE', #1997, .T. ) ;
#6581 =( NAMED_UNIT ( * ) SI_UNIT ( $, .STERADIAN. ) SOLID_ANGLE_UNIT ( ) );
#6582 = CARTESIAN_POINT ( 'NONE',  ( -31.00000000000000000, 19.00000000000000000, -31.00000000000000000 ) ) ;
#6583 = CARTESIAN_POINT ( 'NONE',  ( 0.000000000000000000, 38.00000000000000711, 0.9999999999999943379 ) ) ;
#6584 = ORIENTED_EDGE ( 'NONE', *, *, #11176, .T. ) ;
#6585 = AXIS2_PLACEMENT_3D ( 'NONE', #15688, #13208, #15302 ) ;
#6586 = CARTESIAN_POINT ( 'NONE',  ( 31.00000000000000000, 11.00000000000000000, -31.00000000000000355 ) ) ;
#6587 = FACE_BOUND ( 'NONE', #2658, .T. ) ;
#6588 = EDGE_LOOP ( 'NONE', ( #4596, #16232, #10639, #10044, #16862, #6464, #4612, #11028 ) ) ;
#6589 = CARTESIAN_POINT ( 'NONE',  ( -23.00000000000002487, 10.00000000000000000, -31.00000000000003553 ) ) ;
#6590 = DIRECTION ( 'NONE',  ( -0.000000000000000000, -0.000000000000000000, 1.000000000000000000 ) ) ;
#6591 = VECTOR ( 'NONE', #11545, 1000.000000000000000 ) ;
#6592 = EDGE_CURVE ( 'NONE', #16870, #2442, #8702, .T. ) ;
#6593 = DIRECTION ( 'NONE',  ( 0.000000000000000000, 0.000000000000000000, -1.000000000000000000 ) ) ;
#6594 = ORIENTED_EDGE ( 'NONE', *, *, #42, .T. ) ;
#6595 = CARTESIAN_POINT ( 'NONE',  ( -26.00000000000002842, 3.000000000000000000, 34.00000000000000711 ) ) ;
#6596 = DIRECTION ( 'NONE',  ( -1.000000000000000000, -0.000000000000000000, -0.000000000000000000 ) ) ;
#6597 = CARTESIAN_POINT ( 'NONE',  ( 35.00000000000000711, 0.000000000000000000, 35.00000000000000711 ) ) ;
#6598 = VERTEX_POINT ( 'NONE', #12638 ) ;
#6599 = SURFACE_STYLE_USAGE ( .BOTH. , #4222 ) ;
#6600 = VERTEX_POINT ( 'NONE', #16498 ) ;
#6601 = VERTEX_POINT ( 'NONE', #1046 ) ;
#6602 = DIRECTION ( 'NONE',  ( 0.000000000000000000, 0.000000000000000000, 1.000000000000000000 ) ) ;
#6603 = PRODUCT_DEFINITION ( 'UNKNOWN', '', #11646, #10722 ) ;
#6604 = ORIENTED_EDGE ( 'NONE', *, *, #7944, .T. ) ;
#6605 = ORIENTED_EDGE ( 'NONE', *, *, #2752, .F. ) ;
#6606 = DIRECTION ( 'NONE',  ( 0.000000000000000000, 0.000000000000000000, 1.000000000000000000 ) ) ;
#6607 = AXIS2_PLACEMENT_3D ( 'NONE', #7144, #9910, #15321 ) ;
#6608 = ORIENTED_EDGE ( 'NONE', *, *, #12249, .T. ) ;
#6609 = VECTOR ( 'NONE', #14254, 1000.000000000000000 ) ;
#6610 = ORIENTED_EDGE ( 'NONE', *, *, #1942, .T. ) ;
#6611 = CIRCLE ( 'NONE', #6891, 59.99999999999994316 ) ;
#6612 =( GEOMETRIC_REPRESENTATION_CONTEXT ( 3 ) GLOBAL_UNCERTAINTY_ASSIGNED_CONTEXT ( ( #15342 ) ) GLOBAL_UNIT_ASSIGNED_CONTEXT ( ( #15168, #13795, #3408 ) ) REPRESENTATION_CONTEXT ( 'NONE', 'WORKASPACE' ) );
#6613 = FACE_OUTER_BOUND ( 'NONE', #11458, .T. ) ;
#6614 = CARTESIAN_POINT ( 'NONE',  ( -31.00000000000006750, 0.000000000000000000, 26.00000000000000355 ) ) ;
#6615 = ORIENTED_EDGE ( 'NONE', *, *, #15781, .F. ) ;
#6616 = LINE ( 'NONE', #6447, #8600 ) ;
#6617 = CARTESIAN_POINT ( 'NONE',  ( 1.551310349710149916E-12, 193.2912851029697947, 37.48264153682136168 ) ) ;
#6618 = EDGE_LOOP ( 'NONE', ( #11767, #10206, #11073, #6296 ) ) ;
#6619 = TOROIDAL_SURFACE ( 'NONE', #3629, 4.695405383895982609, 9.000000000000000000 ) ;
#6620 = LINE ( 'NONE', #15650, #642 ) ;
#6621 = ORIENTED_EDGE ( 'NONE', *, *, #16093, .T. ) ;
#6622 = CYLINDRICAL_SURFACE ( 'NONE', #8436, 3.300000000000011369 ) ;
#6623 = CARTESIAN_POINT ( 'NONE',  ( 394.0000000000001137, 339.3157724647196005, -10.68226574335978718 ) ) ;
#6624 = ORIENTED_EDGE ( 'NONE', *, *, #7758, .F. ) ;
#6625 = EDGE_CURVE ( 'NONE', #16672, #7289, #14101, .T. ) ;
#6626 = MECHANICAL_DESIGN_GEOMETRIC_PRESENTATION_REPRESENTATION (  '', ( #8568 ), #6343 ) ;
#6627 = CARTESIAN_POINT ( 'NONE',  ( -23.00000000000002487, 10.00000000000000000, -31.00000000000003553 ) ) ;
#6628 = ORIENTED_EDGE ( 'NONE', *, *, #10323, .F. ) ;
#6629 = CARTESIAN_POINT ( 'NONE',  ( 25.99999999999998224, 10.00000000000000000, -31.00000000000003197 ) ) ;
#6630 = ORIENTED_EDGE ( 'NONE', *, *, #6284, .T. ) ;
#6631 = CIRCLE ( 'NONE', #631, 13.69540538389601991 ) ;
#6632 = EDGE_CURVE ( 'NONE', #15841, #10304, #4902, .T. ) ;
#6633 = ORIENTED_EDGE ( 'NONE', *, *, #3109, .T. ) ;
#6634 = EDGE_CURVE ( 'NONE', #12025, #3926, #4728, .T. ) ;
#6635 = CARTESIAN_POINT ( 'NONE',  ( 0.000000000000000000, 240.7889724647196488, -17.15546574335979813 ) ) ;
#6636 = DIRECTION ( 'NONE',  ( 0.000000000000000000, 0.000000000000000000, -1.000000000000000000 ) ) ;
#6637 = AXIS2_PLACEMENT_3D ( 'NONE', #6122, #11124, #9919 ) ;
#6638 = EDGE_LOOP ( 'NONE', ( #4031, #2471 ) ) ;
#6639 = LINE ( 'NONE', #15927, #14594 ) ;
#6640 = AXIS2_PLACEMENT_3D ( 'NONE', #744, #9844, #8470 ) ;
#6641 = CIRCLE ( 'NONE', #12147, 5.000000000000000888 ) ;
#6642 = CARTESIAN_POINT ( 'NONE',  ( 0.000000000000000000, 376.0487089519837127, -150.0000000000033538 ) ) ;
#6643 = DIRECTION ( 'NONE',  ( -6.123031769111888756E-17, 1.000000000000000000, 3.749151804555346336E-33 ) ) ;
#6644 =( REPRESENTATION_RELATIONSHIP ('NONE','NONE', #15277, #15822 ) REPRESENTATION_RELATIONSHIP_WITH_TRANSFORMATION ( #6501 )SHAPE_REPRESENTATION_RELATIONSHIP( ) );
#6645 = DIRECTION ( 'NONE',  ( -0.000000000000000000, 1.000000000000000000, -0.000000000000000000 ) ) ;
#6646 = LINE ( 'NONE', #9330, #5549 ) ;
#6647 = VECTOR ( 'NONE', #7405, 1000.000000000000000 ) ;
#6648 = EDGE_CURVE ( 'NONE', #5238, #11999, #13852, .T. ) ;
#6649 = CARTESIAN_POINT ( 'NONE',  ( -45.00000000000000000, 493.2350855268092573, -598.9613477082210693 ) ) ;
#6650 = PLANE ( 'NONE',  #9886 ) ;
#6652 = ORIENTED_EDGE ( 'NONE', *, *, #11590, .T. ) ;
#6651 = VERTEX_POINT ( 'NONE', #3623 ) ;
#6653 = VECTOR ( 'NONE', #1581, 1000.000000000000000 ) ;
#6654 = DIRECTION ( 'NONE',  ( -1.000000000000000000, 0.000000000000000000, 1.196361017915039732E-16 ) ) ;
#6655 = VECTOR ( 'NONE', #16543, 1000.000000000000000 ) ;
#6656 = VECTOR ( 'NONE', #12016, 1000.000000000000000 ) ;
#6657 = AXIS2_PLACEMENT_3D ( 'NONE', #6170, #16260, #12621 ) ;
#6658 = AXIS2_PLACEMENT_3D ( 'NONE', #11138, #16538, #915 ) ;
#6659 = EDGE_CURVE ( 'NONE', #4981, #14719, #6441, .T. ) ;
#6660 = EDGE_CURVE ( 'NONE', #12540, #15586, #2078, .T. ) ;
#6661 = EDGE_CURVE ( 'NONE', #14614, #6773, #10152, .T. ) ;
#6662 = EDGE_CURVE ( 'NONE', #7948, #12991, #16376, .T. ) ;
#6663 = CARTESIAN_POINT ( 'NONE',  ( 394.0000000000001137, 240.0523724647196389, -104.2090657433598011 ) ) ;
#6664 = EDGE_CURVE ( 'NONE', #13185, #5045, #7865, .T. ) ;
#6665 = CARTESIAN_POINT ( 'NONE',  ( 45.00000000000000000, 493.2350855268086320, -508.1801094700848580 ) ) ;
#6666 = FACE_OUTER_BOUND ( 'NONE', #16209, .T. ) ;
#6667 = AXIS2_PLACEMENT_3D ( 'NONE', #188, #5582, #8333 ) ;
#6668 = VERTEX_POINT ( 'NONE', #12558 ) ;
#6669 = DIRECTION ( 'NONE',  ( 0.000000000000000000, 0.000000000000000000, 1.000000000000000000 ) ) ;
#6670 = CIRCLE ( 'NONE', #14370, 6.473200000000002063 ) ;
#6671 = AXIS2_PLACEMENT_3D ( 'NONE', #13456, #4269, #9502 ) ;
#6672 = CYLINDRICAL_SURFACE ( 'NONE', #11154, 25.00000000000002132 ) ;
#6673 = EDGE_LOOP ( 'NONE', ( #7900, #8761, #869, #3591 ) ) ;
#6674 = DIRECTION ( 'NONE',  ( 1.000000000000000000, 0.000000000000000000, 0.000000000000000000 ) ) ;
#6675 = AXIS2_PLACEMENT_3D ( 'NONE', #14120, #8795, #7570 ) ;
#6676 = LINE ( 'NONE', #168, #4019 ) ;
#6677 = DIRECTION ( 'NONE',  ( 0.000000000000000000, 0.000000000000000000, -1.000000000000000000 ) ) ;
#6678 = VECTOR ( 'NONE', #14359, 1000.000000000000000 ) ;
#6679 = DIRECTION ( 'NONE',  ( -0.000000000000000000, -1.000000000000000000, 0.000000000000000000 ) ) ;
#6680 = CARTESIAN_POINT ( 'NONE',  ( 10.00000000000000000, 411.2412070270587492, -605.3473189749742005 ) ) ;
#6681 = CARTESIAN_POINT ( 'NONE',  ( -33.99999999999997158, 0.000000000000000000, 31.00000000000000000 ) ) ;
#6682 = ORIENTED_EDGE ( 'NONE', *, *, #9472, .T. ) ;
#6683 = TOROIDAL_SURFACE ( 'NONE', #8623, 22.46376988133006236, 4.000164074322307250 ) ;
#6684 = LINE ( 'NONE', #5986, #4260 ) ;
#6685 = CARTESIAN_POINT ( 'NONE',  ( 0.000000000000000000, 339.4485271457185718, -110.7359021160857537 ) ) ;
#6686 = EDGE_CURVE ( 'NONE', #15220, #7960, #965, .T. ) ;
#6687 = CIRCLE ( 'NONE', #16303, 5.000000000000004441 ) ;
#6688 = DIRECTION ( 'NONE',  ( 0.000000000000000000, 0.000000000000000000, 1.000000000000000000 ) ) ;
#6689 = ORIENTED_EDGE ( 'NONE', *, *, #13807, .F. ) ;
#6690 = AXIS2_PLACEMENT_3D ( 'NONE', #16659, #10310, #2569 ) ;
#6691 = DIRECTION ( 'NONE',  ( 0.000000000000000000, 0.000000000000000000, 1.000000000000000000 ) ) ;
#6692 = FACE_OUTER_BOUND ( 'NONE', #13671, .T. ) ;
#6693 = LINE ( 'NONE', #11948, #6182 ) ;
#6694 = ORIENTED_EDGE ( 'NONE', *, *, #14147, .T. ) ;
#6695 = CARTESIAN_POINT ( 'NONE',  ( 0.000000000000000000, 240.7889724647196488, -104.9456657433598110 ) ) ;
#6696 = DIRECTION ( 'NONE',  ( -1.000000000000000000, -0.000000000000000000, -0.000000000000000000 ) ) ;
#6697 = PLANE ( 'NONE',  #3491 ) ;
#6698 = ORIENTED_EDGE ( 'NONE', *, *, #8456, .T. ) ;
#6699 = AXIS2_PLACEMENT_3D ( 'NONE', #20, #3981, #12127 ) ;
#6700 = DIRECTION ( 'NONE',  ( 0.000000000000000000, 0.000000000000000000, -1.000000000000000000 ) ) ;
#6701 = VECTOR ( 'NONE', #2196, 1000.000000000000000 ) ;
#6702 = EDGE_CURVE ( 'NONE', #6319, #13922, #12500, .T. ) ;
#6703 = ORIENTED_EDGE ( 'NONE', *, *, #7376, .F. ) ;
#6704 = EDGE_LOOP ( 'NONE', ( #3469, #6798, #3354, #2011, #8197, #16598, #9567, #217, #3187, #9397, #11878, #7915, #14610, #10500, #8439, #14064, #6573, #2904, #7228, #16325, #7473, #14081, #16069, #13706, #11699, #16353, #13444, #6511 ) ) ;
#6705 = CARTESIAN_POINT ( 'NONE',  ( 10.00000000000000000, 376.0487089519837127, -150.0000000000033538 ) ) ;
#6706 = TOROIDAL_SURFACE ( 'NONE', #15493, 4.695405383895982609, 9.000000000000000000 ) ;
#6707 = ORIENTED_EDGE ( 'NONE', *, *, #14571, .F. ) ;
#6708 = PRODUCT_CONTEXT ( 'NONE', #16199, 'mechanical' ) ;
#6709 = VERTEX_POINT ( 'NONE', #6184 ) ;
#6710 = ORIENTED_EDGE ( 'NONE', *, *, #15070, .T. ) ;
#6711 = CARTESIAN_POINT ( 'NONE',  ( 39.41161623800082481, 323.9612906317821057, 0.000000000000000000 ) ) ;
#6712 = DIRECTION ( 'NONE',  ( 0.000000000000000000, 1.000000000000000000, 0.000000000000000000 ) ) ;
#6713 = LINE ( 'NONE', #13255, #9450 ) ;
#6714 = ORIENTED_EDGE ( 'NONE', *, *, #1654, .F. ) ;
#6715 = VECTOR ( 'NONE', #5102, 1000.000000000000000 ) ;
#6716 = CARTESIAN_POINT ( 'NONE',  ( 0.000000000000000000, 66.00000000000000000, -9.500000000000000000 ) ) ;
#6717 = FACE_OUTER_BOUND ( 'NONE', #13354, .T. ) ;
#6718 = EDGE_LOOP ( 'NONE', ( #11520, #127, #5375, #12417, #3195, #8306, #16167, #13858, #9016, #10153, #6823, #1263, #7091, #11266, #15363, #5086 ) ) ;
#6719 = CARTESIAN_POINT ( 'NONE',  ( 37.18009836720079875, 352.3758082234937206, -17.00000000000000000 ) ) ;
#6720 = ORIENTED_EDGE ( 'NONE', *, *, #7546, .T. ) ;
#6721 = LINE ( 'NONE', #11975, #12001 ) ;
#6722 = CARTESIAN_POINT ( 'NONE',  ( -30.99999999999999645, 68.00000000000000000, -30.99999999999999289 ) ) ;
#6723 = VERTEX_POINT ( 'NONE', #9821 ) ;
#6724 = DIRECTION ( 'NONE',  ( -1.631319816340925300E-17, 0.000000000000000000, 1.000000000000000000 ) ) ;
#6725 = VERTEX_POINT ( 'NONE', #11436 ) ;
#6726 = CARTESIAN_POINT ( 'NONE',  ( -20.99999999999999645, 19.00000000000000000, 35.00000000000001421 ) ) ;
#6727 = VECTOR ( 'NONE', #5258, 1000.000000000000000 ) ;
#6728 = ORIENTED_EDGE ( 'NONE', *, *, #16865, .T. ) ;
#6729 = ORIENTED_EDGE ( 'NONE', *, *, #7641, .F. ) ;
#6730 = SURFACE_STYLE_FILL_AREA ( #2704 ) ;
#6731 = CYLINDRICAL_SURFACE ( 'NONE', #3604, 12.00000000000000178 ) ;
#6732 = DIRECTION ( 'NONE',  ( -1.000000000000000000, -0.000000000000000000, -0.000000000000000000 ) ) ;
#6733 = ORIENTED_EDGE ( 'NONE', *, *, #6234, .F. ) ;
#6734 = ADVANCED_FACE ( 'NONE', ( #721 ), #5944, .F. ) ;
#6735 = DIRECTION ( 'NONE',  ( 1.000000000000000000, -0.000000000000000000, 0.000000000000000000 ) ) ;
#6736 = DIRECTION ( 'NONE',  ( -0.000000000000000000, -0.000000000000000000, 1.000000000000000000 ) ) ;
#6737 = VECTOR ( 'NONE', #2309, 1000.000000000000000 ) ;
#6738 = DIRECTION ( 'NONE',  ( -0.000000000000000000, -1.000000000000000000, -0.000000000000000000 ) ) ;
#6739 = AXIS2_PLACEMENT_3D ( 'NONE', #249, #10632, #16129 ) ;
#6740 = FACE_OUTER_BOUND ( 'NONE', #1987, .T. ) ;
#6741 = DIRECTION ( 'NONE',  ( 0.000000000000000000, 0.9271838545667883125, 0.3746065934159095168 ) ) ;
#6742 = EDGE_CURVE ( 'NONE', #13922, #12156, #12981, .T. ) ;
#6743 = DIRECTION ( 'NONE',  ( 1.000000000000000000, 0.000000000000000000, 0.000000000000000000 ) ) ;
#6745 = VERTEX_POINT ( 'NONE', #3793 ) ;
#6744 = ORIENTED_EDGE ( 'NONE', *, *, #16868, .T. ) ;
#6746 = LINE ( 'NONE', #4017, #436 ) ;
#6747 = AXIS2_PLACEMENT_3D ( 'NONE', #12095, #335, #14588 ) ;
#6748 = DIRECTION ( 'NONE',  ( -1.000000000000000000, -0.000000000000000000, -0.000000000000000000 ) ) ;
#6749 = VECTOR ( 'NONE', #7132, 1000.000000000000000 ) ;
#6750 = FACE_OUTER_BOUND ( 'NONE', #4204, .T. ) ;
#6751 = DIRECTION ( 'NONE',  ( 0.000000000000000000, 0.000000000000000000, 1.000000000000000000 ) ) ;
#6752 = VERTEX_POINT ( 'NONE', #13072 ) ;
#6753 = EDGE_CURVE ( 'NONE', #2354, #6283, #15719, .T. ) ;
#6754 = ADVANCED_FACE ( 'NONE', ( #3713 ), #10, .F. ) ;
#6755 = DIRECTION ( 'NONE',  ( 1.000000000000000000, 6.123233995736972804E-18, -1.353873099427978431E-32 ) ) ;
#6756 = DIRECTION ( 'NONE',  ( -0.000000000000000000, -0.000000000000000000, 1.000000000000000000 ) ) ;
#6757 = EDGE_LOOP ( 'NONE', ( #5948, #2280 ) ) ;
#6758 = PLANE ( 'NONE',  #7400 ) ;
#6759 = ADVANCED_FACE ( 'NONE', ( #15473 ), #10484, .F. ) ;
#6760 = DIRECTION ( 'NONE',  ( -1.000000000000000000, -0.000000000000000000, -0.000000000000000000 ) ) ;
#6761 = DIRECTION ( 'NONE',  ( 0.000000000000000000, 0.000000000000000000, -1.000000000000000000 ) ) ;
#6762 = ADVANCED_FACE ( 'NONE', ( #8948 ), #6697, .T. ) ;
#6763 = EDGE_CURVE ( 'NONE', #9290, #6541, #5080, .T. ) ;
#6764 = ADVANCED_FACE ( 'NONE', ( #5228 ), #9284, .F. ) ;
#6765 = AXIS2_PLACEMENT_3D ( 'NONE', #16705, #1007, #14375 ) ;
#6766 = EDGE_CURVE ( 'NONE', #15101, #14286, #16106, .T. ) ;
#6767 = CARTESIAN_POINT ( 'NONE',  ( -26.00000000000002842, 3.000000000000000000, 34.00000000000000711 ) ) ;
#6768 = DIRECTION ( 'NONE',  ( 1.000000000000000000, 0.000000000000000000, -0.000000000000000000 ) ) ;
#6769 = ORIENTED_EDGE ( 'NONE', *, *, #5861, .T. ) ;
#6770 = CARTESIAN_POINT ( 'NONE',  ( 55.99999999999989342, 549.5810598491746077, -531.8108303813202156 ) ) ;
#6771 = CARTESIAN_POINT ( 'NONE',  ( -30.99999999999999645, 0.000000000000000000, -30.99999999999999289 ) ) ;
#6772 = AXIS2_PLACEMENT_3D ( 'NONE', #13525, #9657, #12234 ) ;
#6773 = VERTEX_POINT ( 'NONE', #15559 ) ;
#6774 = CARTESIAN_POINT ( 'NONE',  ( 394.0000000000001137, 339.3157724647196005, -10.68226574335978718 ) ) ;
#6775 = DIRECTION ( 'NONE',  ( 1.000000000000000000, 0.000000000000000000, 0.000000000000000000 ) ) ;
#6776 = CARTESIAN_POINT ( 'NONE',  ( 55.99999999999989342, 559.9933750504617365, -546.7230258972048205 ) ) ;
#6777 = EDGE_LOOP ( 'NONE', ( #15736, #13849, #16178, #4573 ) ) ;
#6778 = DIRECTION ( 'NONE',  ( 0.000000000000000000, 0.09950371902100227373, 0.9950371902099888199 ) ) ;
#6779 = EDGE_CURVE ( 'NONE', #214, #6601, #2407, .T. ) ;
#6780 = CARTESIAN_POINT ( 'NONE',  ( 0.000000000000000000, 355.3192028797624857, -37.21049682360899169 ) ) ;
#6781 = CARTESIAN_POINT ( 'NONE',  ( 49.99999999999999289, 515.4878487013597805, -546.7230258972048205 ) ) ;
#6782 = ORIENTED_EDGE ( 'NONE', *, *, #14233, .T. ) ;
#6783 = EDGE_CURVE ( 'NONE', #11935, #5229, #1570, .T. ) ;
#6784 = ADVANCED_FACE ( 'NONE', ( #3873 ), #7272, .T. ) ;
#6785 = CARTESIAN_POINT ( 'NONE',  ( 18.99999999999998224, 10.00000000000000000, -39.99999999999999289 ) ) ;
#6786 = ORIENTED_EDGE ( 'NONE', *, *, #4790, .F. ) ;
#6787 = VERTEX_POINT ( 'NONE', #7638 ) ;
#6788 = CARTESIAN_POINT ( 'NONE',  ( 10.00000000000000000, 185.0000000000000284, -206.3519347178565795 ) ) ;
#6789 = ORIENTED_EDGE ( 'NONE', *, *, #8753, .F. ) ;
#6790 = VERTEX_POINT ( 'NONE', #5327 ) ;
#6791 = ORIENTED_EDGE ( 'NONE', *, *, #2895, .T. ) ;
#6792 = DIRECTION ( 'NONE',  ( 1.000000000000000000, 0.000000000000000000, 0.000000000000000000 ) ) ;
#6793 = CARTESIAN_POINT ( 'NONE',  ( 0.3499999999999999778, 18.17500000000000071, 0.000000000000000000 ) ) ;
#6794 = ORIENTED_EDGE ( 'NONE', *, *, #7672, .T. ) ;
#6795 = DIRECTION ( 'NONE',  ( 0.000000000000000000, -1.000000000000000000, 0.000000000000000000 ) ) ;
#6796 = CIRCLE ( 'NONE', #1313, 35.00000000000000711 ) ;
#6797 = CARTESIAN_POINT ( 'NONE',  ( -31.00000000000000000, 19.00000000000000000, -31.00000000000000000 ) ) ;
#6798 = ORIENTED_EDGE ( 'NONE', *, *, #3147, .F. ) ;
#6799 = DIRECTION ( 'NONE',  ( -1.000000000000000000, 0.000000000000000000, -0.000000000000000000 ) ) ;
#6800 = ORIENTED_EDGE ( 'NONE', *, *, #5035, .F. ) ;
#6801 = DIRECTION ( 'NONE',  ( -1.000000000000000000, 0.000000000000000000, 0.000000000000000000 ) ) ;
#6802 = ORIENTED_EDGE ( 'NONE', *, *, #7180, .T. ) ;
#6803 = CARTESIAN_POINT ( 'NONE',  ( -40.00000000000000711, 8.000000000000000000, -19.00000000000000355 ) ) ;
#6804 = ORIENTED_EDGE ( 'NONE', *, *, #1228, .T. ) ;
#6805 = DIRECTION ( 'NONE',  ( 0.7976179040349731242, 0.000000000000000000, 0.6031630618355673379 ) ) ;
#6806 = DIRECTION ( 'NONE',  ( -0.000000000000000000, -1.000000000000000000, 0.000000000000000000 ) ) ;
#6807 = VECTOR ( 'NONE', #4553, 1000.000000000000000 ) ;
#6808 = ORIENTED_EDGE ( 'NONE', *, *, #5335, .T. ) ;
#6809 = ORIENTED_EDGE ( 'NONE', *, *, #7489, .F. ) ;
#6810 = LINE ( 'NONE', #9321, #14319 ) ;
#6811 = EDGE_CURVE ( 'NONE', #13919, #5039, #1296, .T. ) ;
#6812 = DIRECTION ( 'NONE',  ( 0.000000000000000000, 1.000000000000000000, -1.224646799147353207E-16 ) ) ;
#6813 = CARTESIAN_POINT ( 'NONE',  ( -1.734723475976807094E-15, 60.00000000000000711, 6.000000000000000000 ) ) ;
#6814 = CARTESIAN_POINT ( 'NONE',  ( 5.687501635565830327, -12.64907335584850046, 1.549064719741993485E-15 ) ) ;
#6815 = CARTESIAN_POINT ( 'NONE',  ( -39.99999999999997868, 3.000000000000000000, 26.00000000000000355 ) ) ;
#6816 = EDGE_CURVE ( 'NONE', #12703, #5152, #1126, .T. ) ;
#6817 = CARTESIAN_POINT ( 'NONE',  ( 7.000000000000000000, 0.000000000000000000, 0.000000000000000000 ) ) ;
#6818 = LINE ( 'NONE', #16189, #13424 ) ;
#6819 = LINE ( 'NONE', #4175, #11429 ) ;
#6820 = LINE ( 'NONE', #5371, #16508 ) ;
#6821 = PLANE ( 'NONE',  #6134 ) ;
#6822 = DIRECTION ( 'NONE',  ( 0.000000000000000000, 0.000000000000000000, -1.000000000000000000 ) ) ;
#6824 = ORIENTED_EDGE ( 'NONE', *, *, #11517, .F. ) ;
#6823 = ORIENTED_EDGE ( 'NONE', *, *, #11216, .F. ) ;
#6825 = CARTESIAN_POINT ( 'NONE',  ( 30.99999999999995737, 0.000000000000000000, 31.00000000000000000 ) ) ;
#6826 = AXIS2_PLACEMENT_3D ( 'NONE', #13901, #2126, #7356 ) ;
#6827 = CARTESIAN_POINT ( 'NONE',  ( -1.297668147413691297, 288.9751949913465410, 37.61531421653335627 ) ) ;
#6828 = CARTESIAN_POINT ( 'NONE',  ( -21.00000000000002842, 3.000000000000000000, -37.50000000000000000 ) ) ;
#6829 = LINE ( 'NONE', #2809, #11065 ) ;
#6830 = ADVANCED_FACE ( 'NONE', ( #6344 ), #11770, .F. ) ;
#6831 = ORIENTED_EDGE ( 'NONE', *, *, #12230, .F. ) ;
#6832 = DIRECTION ( 'NONE',  ( 1.000000000000000000, 0.000000000000000000, 0.000000000000000000 ) ) ;
#6833 = AXIS2_PLACEMENT_3D ( 'NONE', #15676, #5277, #1344 ) ;
#6834 = CARTESIAN_POINT ( 'NONE',  ( -18.00000000000001421, 10.00000000000000000, 37.00000000000000711 ) ) ;
#6835 = ORIENTED_EDGE ( 'NONE', *, *, #1322, .T. ) ;
#6836 = CARTESIAN_POINT ( 'NONE',  ( -23.00000000000002487, 10.00000000000000000, -31.00000000000003553 ) ) ;
#6837 = DIRECTION ( 'NONE',  ( 0.000000000000000000, 0.000000000000000000, 1.000000000000000000 ) ) ;
#6838 = LINE ( 'NONE', #8313, #16237 ) ;
#6839 = ORIENTED_EDGE ( 'NONE', *, *, #12765, .T. ) ;
#6840 = PRODUCT_DEFINITION_SHAPE ( 'NONE', 'NONE',  #16981 ) ;
#6841 = CARTESIAN_POINT ( 'NONE',  ( -21.00000000000002842, 3.000000000000000000, -34.99999999999999289 ) ) ;
#6842 =( NAMED_UNIT ( * ) SI_UNIT ( $, .STERADIAN. ) SOLID_ANGLE_UNIT ( ) );
#6843 = CARTESIAN_POINT ( 'NONE',  ( -45.00000000000000000, 473.6663340069158039, -575.6402177818052905 ) ) ;
#6844 = EDGE_LOOP ( 'NONE', ( #6105, #12709 ) ) ;
#6845 = DIRECTION ( 'NONE',  ( -1.000000000000000000, -0.000000000000000000, -0.000000000000000000 ) ) ;
#6846 = EDGE_CURVE ( 'NONE', #12430, #2722, #10903, .T. ) ;
#6847 = EDGE_CURVE ( 'NONE', #13380, #884, #101, .T. ) ;
#6848 = CIRCLE ( 'NONE', #3833, 3.300000000000025135 ) ;
#6849 = CARTESIAN_POINT ( 'NONE',  ( 0.000000000000000000, 240.7889724647196488, -16.41886574335980242 ) ) ;
#6850 = VECTOR ( 'NONE', #13028, 1000.000000000000000 ) ;
#6851 = EDGE_CURVE ( 'NONE', #14523, #10388, #12536, .T. ) ;
#6852 = ORIENTED_EDGE ( 'NONE', *, *, #13269, .F. ) ;
#6853 = FACE_OUTER_BOUND ( 'NONE', #10081, .T. ) ;
#6854 = CARTESIAN_POINT ( 'NONE',  ( 31.00000000000004263, 68.00000000000000000, -25.99999999999999645 ) ) ;
#6855 = DIRECTION ( 'NONE',  ( -1.000000000000000000, -0.000000000000000000, -0.000000000000000000 ) ) ;
#6856 = ORIENTED_EDGE ( 'NONE', *, *, #3304, .T. ) ;
#6857 = DIRECTION ( 'NONE',  ( -1.000000000000000000, 0.000000000000000000, 0.000000000000000000 ) ) ;
#6858 = DIRECTION ( 'NONE',  ( 0.000000000000000000, 1.321694076934710402E-16, -1.000000000000000000 ) ) ;
#6859 = DIRECTION ( 'NONE',  ( 0.000000000000000000, 0.000000000000000000, -1.000000000000000000 ) ) ;
#6860 = ORIENTED_EDGE ( 'NONE', *, *, #11376, .F. ) ;
#6861 = AXIS2_PLACEMENT_3D ( 'NONE', #993, #9053, #14042 ) ;
#6862 = CARTESIAN_POINT ( 'NONE',  ( -30.99999999999999645, 68.00000000000000000, -30.99999999999999289 ) ) ;
#6863 = ORIENTED_EDGE ( 'NONE', *, *, #1546, .T. ) ;
#6864 = ORIENTED_EDGE ( 'NONE', *, *, #16335, .F. ) ;
#6865 = CARTESIAN_POINT ( 'NONE',  ( 22.99999999999998224, 0.000000000000000000, -31.00000000000003197 ) ) ;
#6866 = EDGE_CURVE ( 'NONE', #10898, #12736, #8429, .T. ) ;
#6867 = EDGE_LOOP ( 'NONE', ( #7497, #14609, #5914, #13154, #6209 ) ) ;
#6868 = CARTESIAN_POINT ( 'NONE',  ( 224.9999999999999716, -80.19448206127788126, 6.695756197070496185 ) ) ;
#6869 = ORIENTED_EDGE ( 'NONE', *, *, #6014, .F. ) ;
#6870 = EDGE_CURVE ( 'NONE', #10016, #14834, #14867, .T. ) ;
#6871 = ADVANCED_FACE ( 'NONE', ( #446 ), #13334, .T. ) ;
#6872 = VECTOR ( 'NONE', #11296, 1000.000000000000000 ) ;
#6873 = ADVANCED_FACE ( 'NONE', ( #5675 ), #16152, .F. ) ;
#6874 = EDGE_LOOP ( 'NONE', ( #13981, #11018 ) ) ;
#6875 = EDGE_CURVE ( 'NONE', #3545, #5839, #2085, .T. ) ;
#6876 = CARTESIAN_POINT ( 'NONE',  ( 1.050000000000000044, 0.000000000000000000, 0.000000000000000000 ) ) ;
#6877 = DIRECTION ( 'NONE',  ( 0.000000000000000000, 0.9950371902099890420, -0.09950371902099952592 ) ) ;
#6878 = ORIENTED_EDGE ( 'NONE', *, *, #3326, .F. ) ;
#6879 = DIRECTION ( 'NONE',  ( 1.000000000000000000, 2.556703065963791256E-16, 0.000000000000000000 ) ) ;
#6880 = CARTESIAN_POINT ( 'NONE',  ( -55.99999999999989342, 523.2161522479893847, -585.8570079137933817 ) ) ;
#6881 = ORIENTED_EDGE ( 'NONE', *, *, #2362, .F. ) ;
#6882 = VERTEX_POINT ( 'NONE', #4219 ) ;
#6883 = FACE_BOUND ( 'NONE', #12535, .T. ) ;
#6884 = CARTESIAN_POINT ( 'NONE',  ( -30.99999999999999289, 68.00000000000000000, 31.00000000000000000 ) ) ;
#6885 = ORIENTED_EDGE ( 'NONE', *, *, #13083, .T. ) ;
#6886 = CIRCLE ( 'NONE', #5223, 5.000000000000000888 ) ;
#6887 = CARTESIAN_POINT ( 'NONE',  ( -45.00000000000000000, 523.2161522479893847, -590.5524132976893270 ) ) ;
#6888 = ORIENTED_EDGE ( 'NONE', *, *, #3841, .F. ) ;
#6889 =( NAMED_UNIT ( * ) SI_UNIT ( $, .STERADIAN. ) SOLID_ANGLE_UNIT ( ) );
#6890 = CARTESIAN_POINT ( 'NONE',  ( 3.000000000000000000, 41.00000000000000711, 6.000000000000000000 ) ) ;
#6891 = AXIS2_PLACEMENT_3D ( 'NONE', #13480, #12015, #253 ) ;
#6892 = CIRCLE ( 'NONE', #13225, 13.69540538389601991 ) ;
#6893 = ORIENTED_EDGE ( 'NONE', *, *, #1420, .T. ) ;
#6894 = EDGE_CURVE ( 'NONE', #8784, #6948, #2933, .T. ) ;
#6895 = ORIENTED_EDGE ( 'NONE', *, *, #9937, .F. ) ;
#6896 = CARTESIAN_POINT ( 'NONE',  ( 0.000000000000000000, 0.000000000000000000, 0.000000000000000000 ) ) ;
#6897 = EDGE_CURVE ( 'NONE', #10732, #8165, #10833, .T. ) ;
#6898 = CARTESIAN_POINT ( 'NONE',  ( 0.000000000000000000, 339.1725919290087745, -9.945665743359786148 ) ) ;
#6899 = CARTESIAN_POINT ( 'NONE',  ( 0.000000000000000000, 10.00000000000000000, 0.000000000000000000 ) ) ;
#6900 = VECTOR ( 'NONE', #10496, 1000.000000000000000 ) ;
#6901 = DIRECTION ( 'NONE',  ( -1.000000000000000000, 0.000000000000000000, -1.734723475976807094E-15 ) ) ;
#6902 = CARTESIAN_POINT ( 'NONE',  ( -26.00000000000000355, 11.00000000000000000, 31.00000000000003553 ) ) ;
#6903 = VECTOR ( 'NONE', #10613, 1000.000000000000000 ) ;
#6904 = CARTESIAN_POINT ( 'NONE',  ( -31.81980515339462912, 8.000000000000000000, 35.11980515339465825 ) ) ;
#6905 = VECTOR ( 'NONE', #10717, 1000.000000000000000 ) ;
#6906 = DIRECTION ( 'NONE',  ( 1.000000000000000000, 0.000000000000000000, 0.000000000000000000 ) ) ;
#6907 = AXIS2_PLACEMENT_3D ( 'NONE', #3749, #8985, #16697 ) ;
#6908 = CARTESIAN_POINT ( 'NONE',  ( 31.00000000000000711, 68.00000000000000000, -30.99999999999999289 ) ) ;
#6909 = LINE ( 'NONE', #15155, #1164 ) ;
#6910 = LINE ( 'NONE', #4599, #10538 ) ;
#6911 = LINE ( 'NONE', #12171, #1094 ) ;
#6913 = ORIENTED_EDGE ( 'NONE', *, *, #15195, .T. ) ;
#6912 = ORIENTED_EDGE ( 'NONE', *, *, #12545, .T. ) ;
#6914 = AXIS2_PLACEMENT_3D ( 'NONE', #15466, #11432, #7633 ) ;
#6915 = DIRECTION ( 'NONE',  ( -1.000000000000000000, 0.000000000000000000, -0.000000000000000000 ) ) ;
#6916 = DIRECTION ( 'NONE',  ( 0.000000000000000000, 1.000000000000000000, 1.321694076934710402E-16 ) ) ;
#6917 = VECTOR ( 'NONE', #16191, 1000.000000000000000 ) ;
#6918 = VECTOR ( 'NONE', #12283, 1000.000000000000000 ) ;
#6919 = CARTESIAN_POINT ( 'NONE',  ( 56.73000000000001108, 239.4632308570078294, 71.73739990498292229 ) ) ;
#6920 = PLANE ( 'NONE',  #15171 ) ;
#6921 = ORIENTED_EDGE ( 'NONE', *, *, #3967, .F. ) ;
#6922 = CARTESIAN_POINT ( 'NONE',  ( -37.00000000000000000, 68.00000000000000000, -22.99999999999999645 ) ) ;
#6923 = AXIS2_PLACEMENT_3D ( 'NONE', #8500, #5918, #9797 ) ;
#6924 = CARTESIAN_POINT ( 'NONE',  ( 55.99999999999989342, 549.5810598491749488, -570.6352214130889706 ) ) ;
#6925 = VERTEX_POINT ( 'NONE', #273 ) ;
#6926 = DIRECTION ( 'NONE',  ( -0.000000000000000000, -1.000000000000000000, -0.000000000000000000 ) ) ;
#6927 = CARTESIAN_POINT ( 'NONE',  ( -46.99999999999988631, 549.5810598491749488, -575.3306267969850296 ) ) ;
#6928 = CARTESIAN_POINT ( 'NONE',  ( 10.00000000000000000, 0.000000000000000000, 0.000000000000000000 ) ) ;
#6929 = CONICAL_SURFACE ( 'NONE', #15444, 18.17500000000000071, 0.7483780475235185525 ) ;
#6930 = ADVANCED_FACE ( 'NONE', ( #8077 ), #1560, .F. ) ;
#6931 = AXIS2_PLACEMENT_3D ( 'NONE', #1498, #5352, #13267 ) ;
#6932 = DIRECTION ( 'NONE',  ( 0.000000000000000000, 1.000000000000000000, -0.000000000000000000 ) ) ;
#6933 = AXIS2_PLACEMENT_3D ( 'NONE', #9693, #5644, #14839 ) ;
#6934 = DIRECTION ( 'NONE',  ( 0.000000000000000000, -1.000000000000000000, 0.000000000000000000 ) ) ;
#6935 = VERTEX_POINT ( 'NONE', #1640 ) ;
#6936 = LINE ( 'NONE', #6770, #8382 ) ;
#6937 = SHAPE_REPRESENTATION ( 'Servo-Axe', ( #1488 ), #5315 ) ;
#6938 = VECTOR ( 'NONE', #12052, 1000.000000000000000 ) ;
#6939 = CARTESIAN_POINT ( 'NONE',  ( 26.00000000000000355, 11.00000000000000000, -40.00000000000000711 ) ) ;
#6940 =( LENGTH_UNIT ( ) NAMED_UNIT ( * ) SI_UNIT ( .MILLI., .METRE. ) );
#6941 = AXIS2_PLACEMENT_3D ( 'NONE', #9048, #16936, #10171 ) ;
#6942 = VERTEX_POINT ( 'NONE', #11952 ) ;
#6943 = AXIS2_PLACEMENT_3D ( 'NONE', #16703, #2368, #11645 ) ;
#6944 = VECTOR ( 'NONE', #734, 1000.000000000000000 ) ;
#6945 = CARTESIAN_POINT ( 'NONE',  ( -31.81980515339462912, 8.000000000000000000, -31.81980515339465043 ) ) ;
#6946 = ADVANCED_FACE ( 'NONE', ( #11000 ), #4315, .T. ) ;
#6947 = LINE ( 'NONE', #9457, #8938 ) ;
#6948 = VERTEX_POINT ( 'NONE', #6951 ) ;
#6949 = CARTESIAN_POINT ( 'NONE',  ( -26.00000000000002132, 10.00000000000000000, -39.99999999999999289 ) ) ;
#6950 = DIRECTION ( 'NONE',  ( -0.000000000000000000, -1.000000000000000000, -0.000000000000000000 ) ) ;
#6951 = CARTESIAN_POINT ( 'NONE',  ( 0.000000000000000000, 240.7889724647196488, -16.41886574335980242 ) ) ;
#6952 = VERTEX_POINT ( 'NONE', #15884 ) ;
#6953 = CIRCLE ( 'NONE', #392, 13.69540538389601991 ) ;
#6954 = CARTESIAN_POINT ( 'NONE',  ( -46.99999999999988631, 549.5810598491746077, -518.1154249974242703 ) ) ;
#6955 = ORIENTED_EDGE ( 'NONE', *, *, #16425, .T. ) ;
#6956 = ORIENTED_EDGE ( 'NONE', *, *, #4280, .F. ) ;
#6957 = AXIS2_PLACEMENT_3D ( 'NONE', #16836, #6518, #5072 ) ;
#6958 = EDGE_CURVE ( 'NONE', #2938, #14585, #5584, .T. ) ;
#6959 = CARTESIAN_POINT ( 'NONE',  ( -26.00000000000002842, 3.000000000000000000, -39.99999999999999289 ) ) ;
#6960 = VECTOR ( 'NONE', #13517, 1000.000000000000000 ) ;
#6961 = ORIENTED_EDGE ( 'NONE', *, *, #5560, .F. ) ;
#6962 = DIRECTION ( 'NONE',  ( 0.000000000000000000, 0.000000000000000000, 1.000000000000000000 ) ) ;
#6963 = AXIS2_PLACEMENT_3D ( 'NONE', #14831, #1862, #15075 ) ;
#6964 = ORIENTED_EDGE ( 'NONE', *, *, #14837, .T. ) ;
#6965 = VECTOR ( 'NONE', #6076, 1000.000000000000000 ) ;
#6966 = ORIENTED_EDGE ( 'NONE', *, *, #5598, .F. ) ;
#6967 = CARTESIAN_POINT ( 'NONE',  ( -26.00000000000000000, 11.00000000000000000, -40.00000000000000711 ) ) ;
#6968 = CYLINDRICAL_SURFACE ( 'NONE', #8347, 8.000000000000000000 ) ;
#6969 = EDGE_CURVE ( 'NONE', #6598, #3462, #8335, .T. ) ;
#6970 = VERTEX_POINT ( 'NONE', #1891 ) ;
#6971 = CARTESIAN_POINT ( 'NONE',  ( 0.000000000000000000, 339.4485271457185718, -110.7359021160857537 ) ) ;
#6972 = VECTOR ( 'NONE', #12727, 1000.000000000000000 ) ;
#6973 = LINE ( 'NONE', #9566, #5392 ) ;
#6974 = ORIENTED_EDGE ( 'NONE', *, *, #10767, .T. ) ;
#6975 = TOROIDAL_SURFACE ( 'NONE', #1786, 4.695405383895982609, 9.000000000000000000 ) ;
#6976 = EDGE_CURVE ( 'NONE', #11526, #11059, #3014, .T. ) ;
#6977 = ORIENTED_EDGE ( 'NONE', *, *, #11141, .F. ) ;
#6978 = DIRECTION ( 'NONE',  ( 1.000000000000000000, 0.000000000000000000, 0.000000000000000000 ) ) ;
#6979 = CARTESIAN_POINT ( 'NONE',  ( 54.99999999999999289, 515.4878487013597805, -546.7230258972048205 ) ) ;
#6980 = ORIENTED_EDGE ( 'NONE', *, *, #1631, .T. ) ;
#6981 = EDGE_CURVE ( 'NONE', #4216, #3286, #7550, .T. ) ;
#6982 = EDGE_CURVE ( 'NONE', #6651, #6970, #528, .T. ) ;
#6983 = ORIENTED_EDGE ( 'NONE', *, *, #12460, .F. ) ;
#6984 = DIRECTION ( 'NONE',  ( -0.000000000000000000, -1.000000000000000000, -0.000000000000000000 ) ) ;
#6985 = DIRECTION ( 'NONE',  ( -0.000000000000000000, -1.000000000000000000, -0.000000000000000000 ) ) ;
#6986 = ORIENTED_EDGE ( 'NONE', *, *, #2516, .F. ) ;
#6987 =( REPRESENTATION_RELATIONSHIP ('NONE','NONE', #15822, #11211 ) REPRESENTATION_RELATIONSHIP_WITH_TRANSFORMATION ( #4113 )SHAPE_REPRESENTATION_RELATIONSHIP( ) );
#6988 = EDGE_LOOP ( 'NONE', ( #9373, #1616 ) ) ;
#6989 = CARTESIAN_POINT ( 'NONE',  ( -2.600106608147766174, 39.49089379158813529, 9.137947797636652325 ) ) ;
#6990 = CARTESIAN_POINT ( 'NONE',  ( 39.06972645625037899, 346.7108172824755457, -6.736600000000000144 ) ) ;
#6991 = DIRECTION ( 'NONE',  ( -0.000000000000000000, -0.000000000000000000, 1.000000000000000000 ) ) ;
#6992 = PLANE ( 'NONE',  #11738 ) ;
#6993 = PRODUCT_DEFINITION_SHAPE ( 'NONE', 'NONE',  #5043 ) ;
#6994 = CARTESIAN_POINT ( 'NONE',  ( 1.050000000000000044, 0.000000000000000000, 0.000000000000000000 ) ) ;
#6995 = CARTESIAN_POINT ( 'NONE',  ( -1.281199806751482040, 189.9796977361249048, 37.61247111518787989 ) ) ;
#6996 = DIRECTION ( 'NONE',  ( 0.000000000000000000, -1.000000000000000000, 0.000000000000000000 ) ) ;
#6997 = ADVANCED_FACE ( 'NONE', ( #9367 ), #14608, .F. ) ;
#6998 = CARTESIAN_POINT ( 'NONE',  ( 26.00000000000000000, 19.00000000000000000, 40.00000000000001421 ) ) ;
#6999 = LINE ( 'NONE', #4273, #16786 ) ;
#7000 = EDGE_CURVE ( 'NONE', #11956, #8711, #15366, .T. ) ;
#7001 = VECTOR ( 'NONE', #6915, 1000.000000000000000 ) ;
#7002 = EDGE_CURVE ( 'NONE', #14529, #1196, #2137, .T. ) ;
#7003 = DIRECTION ( 'NONE',  ( -1.000000000000000000, -0.000000000000000000, -0.000000000000000000 ) ) ;
#7004 = DIRECTION ( 'NONE',  ( -1.000000000000000000, -0.000000000000000000, 0.000000000000000000 ) ) ;
#7006 = VERTEX_POINT ( 'NONE', #3523 ) ;
#7005 = VERTEX_POINT ( 'NONE', #16478 ) ;
#7007 = PLANE ( 'NONE',  #11943 ) ;
#7008 = PRODUCT ( 'Part4', 'Part4', '', ( #2227 ) ) ;
#7009 = CARTESIAN_POINT ( 'NONE',  ( 35.00000000000000711, 8.000000000000000000, 20.99999999999999289 ) ) ;
#7010 = DIRECTION ( 'NONE',  ( 1.000000000000000000, -0.000000000000000000, 0.000000000000000000 ) ) ;
#7011 = CARTESIAN_POINT ( 'NONE',  ( 1.224999999999999867, 0.000000000000000000, 0.000000000000000000 ) ) ;
#7012 = AXIS2_PLACEMENT_3D ( 'NONE', #4642, #7812, #2665 ) ;
#7013 = EDGE_LOOP ( 'NONE', ( #9535, #12114, #6086, #1247 ) ) ;
#7014 = VECTOR ( 'NONE', #5702, 1000.000000000000000 ) ;
#7015 = CARTESIAN_POINT ( 'NONE',  ( -55.99999999999989342, 473.6663340069157471, -531.5012393965008641 ) ) ;
#7016 = ORIENTED_EDGE ( 'NONE', *, *, #15708, .F. ) ;
#7017 = CARTESIAN_POINT ( 'NONE',  ( -2.980268877975830399, 60.39571231257155404, 9.020512128682495856 ) ) ;
#7018 = CARTESIAN_POINT ( 'NONE',  ( -55.99999999999989342, 559.9933750504617365, -560.4184312811007658 ) ) ;
#7019 = FACE_BOUND ( 'NONE', #11134, .T. ) ;
#7020 = CARTESIAN_POINT ( 'NONE',  ( 30.99999999999999645, 3.000000000000000000, -25.99999999999999645 ) ) ;
#7021 = ORIENTED_EDGE ( 'NONE', *, *, #194, .F. ) ;
#7022 = AXIS2_PLACEMENT_3D ( 'NONE', #10213, #3944, #13049 ) ;
#7023 = DIRECTION ( 'NONE',  ( -1.000000000000000000, -0.000000000000000000, -0.000000000000000000 ) ) ;
#7024 = AXIS2_PLACEMENT_3D ( 'NONE', #3518, #2133, #9876 ) ;
#7025 = DIRECTION ( 'NONE',  ( 0.000000000000000000, 0.000000000000000000, 1.000000000000000000 ) ) ;
#7026 = CARTESIAN_POINT ( 'NONE',  ( 25.99999999999999645, 68.00000000000000000, 40.00000000000002132 ) ) ;
#7027 = EDGE_LOOP ( 'NONE', ( #13477, #192, #14781, #11541 ) ) ;
#7028 = FACE_BOUND ( 'NONE', #15045, .T. ) ;
#7029 = EDGE_CURVE ( 'NONE', #16672, #12012, #3602, .T. ) ;
#7030 = AXIS2_PLACEMENT_3D ( 'NONE', #11815, #3761, #3587 ) ;
#7031 = CARTESIAN_POINT ( 'NONE',  ( -45.00000000000000000, 515.4878487013597805, -486.7230258972047636 ) ) ;
#7032 = ORIENTED_EDGE ( 'NONE', *, *, #4132, .T. ) ;
#7033 = AXIS2_PLACEMENT_3D ( 'NONE', #13259, #10674, #4862 ) ;
#7034 = DIRECTION ( 'NONE',  ( 1.000000000000000000, 0.000000000000000000, 0.000000000000000000 ) ) ;
#7035 = CARTESIAN_POINT ( 'NONE',  ( -430.0000000000000568, 620.7506394335853201, 0.000000000000000000 ) ) ;
#7036 = CARTESIAN_POINT ( 'NONE',  ( 0.000000000000000000, -3.000000000000000000, 35.00000000000000711 ) ) ;
#7037 = EDGE_LOOP ( 'NONE', ( #1901, #5739 ) ) ;
#7038 = DIRECTION ( 'NONE',  ( -0.000000000000000000, -1.000000000000000000, -0.000000000000000000 ) ) ;
#7039 = VERTEX_POINT ( 'NONE', #9967 ) ;
#7040 = VERTEX_POINT ( 'NONE', #6078 ) ;
#7041 = FACE_OUTER_BOUND ( 'NONE', #7618, .T. ) ;
#7042 = ORIENTED_EDGE ( 'NONE', *, *, #16609, .F. ) ;
#7043 = VECTOR ( 'NONE', #13094, 1000.000000000000000 ) ;
#7044 = PRODUCT_RELATED_PRODUCT_CATEGORY ( 'part', '', ( #440 ) ) ;
#7045 = EDGE_LOOP ( 'NONE', ( #1357, #6163, #9198, #12871 ) ) ;
#7046 = CARTESIAN_POINT ( 'NONE',  ( 0.000000000000000000, 372.8685141053783241, -143.5198051533979537 ) ) ;
#7047 = EDGE_LOOP ( 'NONE', ( #2106, #3628, #3718, #3578, #3077 ) ) ;
#7048 = DIRECTION ( 'NONE',  ( 1.000000000000000000, -0.000000000000000000, -0.000000000000000000 ) ) ;
#7049 = DIRECTION ( 'NONE',  ( 0.000000000000000000, -1.000000000000000000, 0.000000000000000000 ) ) ;
#7050 = EDGE_CURVE ( 'NONE', #6952, #15054, #11328, .T. ) ;
#7051 = VERTEX_POINT ( 'NONE', #11084 ) ;
#7052 = CARTESIAN_POINT ( 'NONE',  ( -55.99999999999989342, 523.2161522479893847, -590.5524132976893270 ) ) ;
#7053 = CARTESIAN_POINT ( 'NONE',  ( 7.000000000000001776, 380.0000000000000000, -65.00000000000000000 ) ) ;
#7054 = ORIENTED_EDGE ( 'NONE', *, *, #4153, .T. ) ;
#7055 = STYLED_ITEM ( 'NONE', ( #12712 ), #8355 ) ;
#7056 = SURFACE_SIDE_STYLE ('',( #9823 ) ) ;
#7057 = EDGE_LOOP ( 'NONE', ( #14483, #4907, #8310, #13491 ) ) ;
#7058 = LINE ( 'NONE', #13689, #14344 ) ;
#7059 = VERTEX_POINT ( 'NONE', #14080 ) ;
#7060 = ORIENTED_EDGE ( 'NONE', *, *, #8787, .F. ) ;
#7061 = CARTESIAN_POINT ( 'NONE',  ( -19.00000000000001776, 8.000000000000000000, 36.00000000000000711 ) ) ;
#7062 = EDGE_CURVE ( 'NONE', #1606, #14752, #859, .T. ) ;
#7063 = ORIENTED_EDGE ( 'NONE', *, *, #14017, .T. ) ;
#7064 = ORIENTED_EDGE ( 'NONE', *, *, #7394, .T. ) ;
#7065 = CARTESIAN_POINT ( 'NONE',  ( -39.99999999999999289, 11.00000000000000000, -34.99999999999997868 ) ) ;
#7066 = AXIS2_PLACEMENT_3D ( 'NONE', #16067, #11769, #3968 ) ;
#7067 = DIRECTION ( 'NONE',  ( 0.000000000000000000, 0.000000000000000000, 1.000000000000000000 ) ) ;
#7068 = EDGE_CURVE ( 'NONE', #6189, #793, #16078, .T. ) ;
#7069 = DIRECTION ( 'NONE',  ( 1.000000000000000000, 0.000000000000000000, 0.000000000000000000 ) ) ;
#7070 = EDGE_CURVE ( 'NONE', #9593, #10447, #16570, .T. ) ;
#7072 = EDGE_CURVE ( 'NONE', #3136, #8449, #2058, .T. ) ;
#7071 = DIRECTION ( 'NONE',  ( 1.734723475976807094E-15, 0.000000000000000000, -1.000000000000000000 ) ) ;
#7073 = LINE ( 'NONE', #4750, #4498 ) ;
#7074 = CARTESIAN_POINT ( 'NONE',  ( -46.99999999999988631, 523.2161522479888163, -498.1982331128240276 ) ) ;
#7075 = CARTESIAN_POINT ( 'NONE',  ( 10.00000000000000000, 0.000000000000000000, -206.3519347178565795 ) ) ;
#7076 = DIRECTION ( 'NONE',  ( -1.000000000000000000, -0.000000000000000000, 0.000000000000000000 ) ) ;
#7077 = LINE ( 'NONE', #5797, #13782 ) ;
#7078 = DIRECTION ( 'NONE',  ( -1.000000000000000000, -0.000000000000000000, -0.000000000000000000 ) ) ;
#7079 = LINE ( 'NONE', #11130, #15087 ) ;
#7081 = ORIENTED_EDGE ( 'NONE', *, *, #15827, .T. ) ;
#7080 = ORIENTED_EDGE ( 'NONE', *, *, #8262, .F. ) ;
#7082 = APPLICATION_CONTEXT ( 'automotive_design' ) ;
#7083 = DIRECTION ( 'NONE',  ( 0.000000000000000000, 0.000000000000000000, -1.000000000000000000 ) ) ;
#7084 = ADVANCED_FACE ( 'NONE', ( #4554 ), #5838, .T. ) ;
#7085 = ITEM_DEFINED_TRANSFORMATION ( 'NONE', 'NONE', #14930,  #1488 ) ;
#7086 = CYLINDRICAL_SURFACE ( 'NONE', #15929, 13.69540538389601991 ) ;
#7087 = ADVANCED_FACE ( 'NONE', ( #5923 ), #7445, .F. ) ;
#7088 = PLANE ( 'NONE',  #10505 ) ;
#7089 = EDGE_CURVE ( 'NONE', #15120, #15290, #3467, .T. ) ;
#7091 = ORIENTED_EDGE ( 'NONE', *, *, #1916, .F. ) ;
#7090 = EDGE_CURVE ( 'NONE', #6600, #5722, #12372, .T. ) ;
#7092 = ADVANCED_FACE ( 'NONE', ( #7288 ), #5997, .T. ) ;
#7093 = VECTOR ( 'NONE', #13705, 1000.000000000000000 ) ;
#7094 = FACE_OUTER_BOUND ( 'NONE', #3182, .T. ) ;
#7095 = ORIENTED_EDGE ( 'NONE', *, *, #4037, .F. ) ;
#7096 = CARTESIAN_POINT ( 'NONE',  ( 4.025000000000000355, 0.000000000000000000, 0.000000000000000000 ) ) ;
#7097 = CARTESIAN_POINT ( 'NONE',  ( -0.3206782292910441146, 189.5419480837538231, 37.58913636098570521 ) ) ;
#7098 = DIRECTION ( 'NONE',  ( 0.000000000000000000, 0.000000000000000000, 1.000000000000000000 ) ) ;
#7099 = AXIS2_PLACEMENT_3D ( 'NONE', #1423, #6643, #10696 ) ;
#7100 = CARTESIAN_POINT ( 'NONE',  ( 21.99999999999998224, 6.000000000000000000, -35.99999999999999289 ) ) ;
#7101 = PRESENTATION_STYLE_ASSIGNMENT (( #12017 ) ) ;
#7102 = VERTEX_POINT ( 'NONE', #16323 ) ;
#7103 = DIRECTION ( 'NONE',  ( 1.000000000000000000, -0.000000000000000000, 0.000000000000000000 ) ) ;
#7104 = CYLINDRICAL_SURFACE ( 'NONE', #11504, 13.69540538389601991 ) ;
#7105 = CYLINDRICAL_SURFACE ( 'NONE', #5005, 22.50000000000000000 ) ;
#7106 = VECTOR ( 'NONE', #13323, 1000.000000000000000 ) ;
#7107 = ORIENTED_EDGE ( 'NONE', *, *, #4237, .T. ) ;
#7108 = ADVANCED_FACE ( 'NONE', ( #16652 ), #3441, .F. ) ;
#7109 = DIRECTION ( 'NONE',  ( 0.000000000000000000, -1.000000000000000000, 0.000000000000000000 ) ) ;
#7110 = DIRECTION ( 'NONE',  ( 0.9998870921963913805, 0.01502673813723915709, 0.000000000000000000 ) ) ;
#7111 = EDGE_LOOP ( 'NONE', ( #12385, #811, #8622, #13646 ) ) ;
#7112 = FACE_OUTER_BOUND ( 'NONE', #14395, .T. ) ;
#7113 = DIRECTION ( 'NONE',  ( 0.000000000000000000, 0.000000000000000000, 1.000000000000000000 ) ) ;
#7114 = DIRECTION ( 'NONE',  ( 0.000000000000000000, 0.000000000000000000, -1.000000000000000000 ) ) ;
#7115 = ORIENTED_EDGE ( 'NONE', *, *, #2028, .F. ) ;
#7116 = ORIENTED_EDGE ( 'NONE', *, *, #16223, .F. ) ;
#7117 = EDGE_LOOP ( 'NONE', ( #6287, #288 ) ) ;
#7118 = AXIS2_PLACEMENT_3D ( 'NONE', #8294, #13379, #11998 ) ;
#7119 = LINE ( 'NONE', #11091, #10279 ) ;
#7120 = EDGE_CURVE ( 'NONE', #11290, #16915, #8120, .T. ) ;
#7121 = APPLICATION_PROTOCOL_DEFINITION ( 'draft international standard', 'automotive_design', 1998, #1071 ) ;
#7122 = CIRCLE ( 'NONE', #13188, 3.000000000000002665 ) ;
#7123 = VERTEX_POINT ( 'NONE', #12456 ) ;
#7124 = CARTESIAN_POINT ( 'NONE',  ( 75.00000000000000000, 380.0000000000000000, 0.000000000000000000 ) ) ;
#7125 = ORIENTED_EDGE ( 'NONE', *, *, #8132, .F. ) ;
#7126 = LINE ( 'NONE', #12383, #1145 ) ;
#7127 = DIRECTION ( 'NONE',  ( 1.000000000000000000, -0.000000000000000000, 0.000000000000000000 ) ) ;
#7128 = VECTOR ( 'NONE', #3653, 1000.000000000000000 ) ;
#7129 = ORIENTED_EDGE ( 'NONE', *, *, #16630, .F. ) ;
#7131 = FACE_OUTER_BOUND ( 'NONE', #9143, .T. ) ;
#7130 = AXIS2_PLACEMENT_3D ( 'NONE', #819, #16188, #8541 ) ;
#7132 = DIRECTION ( 'NONE',  ( 1.000000000000000000, -3.400581542615706812E-15, 2.422066625794662531E-16 ) ) ;
#7133 = ORIENTED_EDGE ( 'NONE', *, *, #16207, .F. ) ;
#7134 = COLOUR_RGB ( '', 0.66274510, 0.83137255, 0.94901961) ;
#7135 = VECTOR ( 'NONE', #12410, 1000.000000000000000 ) ;
#7136 = DIRECTION ( 'NONE',  ( -0.000000000000000000, -1.000000000000000000, -0.000000000000000000 ) ) ;
#7137 = ORIENTED_EDGE ( 'NONE', *, *, #13970, .T. ) ;
#7138 = ORIENTED_EDGE ( 'NONE', *, *, #13074, .F. ) ;
#7139 = ORIENTED_EDGE ( 'NONE', *, *, #15479, .T. ) ;
#7140 = VECTOR ( 'NONE', #7163, 1000.000000000000000 ) ;
#7141 = ORIENTED_EDGE ( 'NONE', *, *, #7826, .T. ) ;
#7142 = ORIENTED_EDGE ( 'NONE', *, *, #2362, .T. ) ;
#7143 = DIRECTION ( 'NONE',  ( 1.000000000000000000, 0.000000000000000000, -0.000000000000000000 ) ) ;
#7144 = CARTESIAN_POINT ( 'NONE',  ( -46.99999999999988631, 549.5810598491749488, -580.0260321808809749 ) ) ;
#7145 = DIRECTION ( 'NONE',  ( 9.736587334121946093E-17, 0.09950371902099953980, 0.9950371902099891530 ) ) ;
#7146 = CARTESIAN_POINT ( 'NONE',  ( -1.734723475976807094E-15, 60.00000000000000711, 6.000000000000000000 ) ) ;
#7147 = DIRECTION ( 'NONE',  ( -8.673617379884027583E-16, 0.000000000000000000, 1.000000000000000000 ) ) ;
#7148 = ADVANCED_FACE ( 'NONE', ( #8932, #7621 ), #14251, .T. ) ;
#7149 = CARTESIAN_POINT ( 'NONE',  ( 10.00000000000000000, 381.0487089519837127, -150.0000000000032685 ) ) ;
#7150 = PLANE ( 'NONE',  #6637 ) ;
#7151 = ORIENTED_EDGE ( 'NONE', *, *, #12980, .T. ) ;
#7152 = LINE ( 'NONE', #15329, #5121 ) ;
#7153 = LINE ( 'NONE', #9682, #4470 ) ;
#7154 = AXIS2_PLACEMENT_3D ( 'NONE', #7539, #6679, #10557 ) ;
#7155 = CLOSED_SHELL ( 'NONE', ( #5282, #1284, #12567, #13700, #5933, #12130, #309, #1079, #7171, #2897, #15658, #14881, #12858, #2654, #6141, #12282, #6336, #5784, #7911, #6784, #16658, #1940, #6548, #8684, #11155, #4322, #6374, #8234, #11716, #12770, #9936, #503, #11584 ) ) ;
#7156 = DIRECTION ( 'NONE',  ( 1.000000000000000000, 0.000000000000000000, 0.000000000000000000 ) ) ;
#7157 = DIRECTION ( 'NONE',  ( 0.000000000000000000, 0.000000000000000000, 1.000000000000000000 ) ) ;
#7159 = ORIENTED_EDGE ( 'NONE', *, *, #12644, .T. ) ;
#7158 = EDGE_LOOP ( 'NONE', ( #16674, #8023, #8733, #15161, #12742, #731 ) ) ;
#7160 = EDGE_CURVE ( 'NONE', #15552, #16255, #14170, .T. ) ;
#7161 = CARTESIAN_POINT ( 'NONE',  ( 40.00000000000000000, 0.000000000000000000, 26.00000000000000355 ) ) ;
#7162 = PRESENTATION_STYLE_ASSIGNMENT (( #1941 ) ) ;
#7163 = DIRECTION ( 'NONE',  ( -1.000000000000000000, -0.000000000000000000, -0.000000000000000000 ) ) ;
#7164 = CARTESIAN_POINT ( 'NONE',  ( -55.99999999999989342, 523.2161522479893847, -590.5524132976893270 ) ) ;
#7165 = EDGE_LOOP ( 'NONE', ( #15474, #2851, #12769, #2393 ) ) ;
#7166 = VECTOR ( 'NONE', #11900, 1000.000000000000000 ) ;
#7167 = CIRCLE ( 'NONE', #7448, 0.7366000000000039183 ) ;
#7168 = DIRECTION ( 'NONE',  ( 0.000000000000000000, -1.000000000000000000, 0.000000000000000000 ) ) ;
#7169 = CARTESIAN_POINT ( 'NONE',  ( 0.5437585709476746576, 192.7236469956751534, 37.27096646979358496 ) ) ;
#7171 = ADVANCED_FACE ( 'NONE', ( #10553 ), #11406, .T. ) ;
#7170 = ORIENTED_EDGE ( 'NONE', *, *, #3346, .T. ) ;
#7172 = CARTESIAN_POINT ( 'NONE',  ( -0.1972064085032595726, 63.00000000000000000, 9.500000000000001776 ) ) ;
#7173 = DIRECTION ( 'NONE',  ( 1.000000000000000000, 0.000000000000000000, 0.000000000000000000 ) ) ;
#7174 = LINE ( 'NONE', #4866, #8567 ) ;
#7175 = AXIS2_PLACEMENT_3D ( 'NONE', #13847, #14009, #7303 ) ;
#7176 = CARTESIAN_POINT ( 'NONE',  ( -39.99999999999999289, 11.00000000000000000, -34.99999999999997868 ) ) ;
#7177 = DIRECTION ( 'NONE',  ( 0.000000000000000000, 0.000000000000000000, -1.000000000000000000 ) ) ;
#7178 = VERTEX_POINT ( 'NONE', #3777 ) ;
#7179 = EDGE_CURVE ( 'NONE', #14967, #1326, #9267, .T. ) ;
#7180 = EDGE_CURVE ( 'NONE', #12818, #16324, #6408, .T. ) ;
#7181 = EDGE_CURVE ( 'NONE', #9156, #614, #2392, .T. ) ;
#7182 = ADVANCED_FACE ( 'NONE', ( #12870 ), #11667, .T. ) ;
#7183 = DIRECTION ( 'NONE',  ( -1.000000000000000000, 0.000000000000000000, -0.000000000000000000 ) ) ;
#7184 = EDGE_CURVE ( 'NONE', #1629, #3161, #7537, .T. ) ;
#7185 = CIRCLE ( 'NONE', #4456, 13.69540538389601991 ) ;
#7186 = CARTESIAN_POINT ( 'NONE',  ( 46.99999999999988631, 559.9933750504617365, -546.7230258972048205 ) ) ;
#7187 = CARTESIAN_POINT ( 'NONE',  ( 30.99999999999999645, 3.000000000000000000, 26.00000000000000355 ) ) ;
#7188 = AXIS2_PLACEMENT_3D ( 'NONE', #11747, #1185, #5205 ) ;
#7189 = VERTEX_POINT ( 'NONE', #6495 ) ;
#7190 = DIRECTION ( 'NONE',  ( -0.000000000000000000, -0.000000000000000000, 1.000000000000000000 ) ) ;
#7191 = DIRECTION ( 'NONE',  ( 1.000000000000000000, -6.123031769111888756E-17, 0.000000000000000000 ) ) ;
#7192 = ORIENTED_EDGE ( 'NONE', *, *, #8848, .F. ) ;
#7193 = DIRECTION ( 'NONE',  ( 0.000000000000000000, 0.000000000000000000, 1.000000000000000000 ) ) ;
#7194 = VECTOR ( 'NONE', #10094, 1000.000000000000114 ) ;
#7195 = COLOUR_RGB ( '', 0.08235294, 0.09019608, 0.10196078) ;
#7196 = CARTESIAN_POINT ( 'NONE',  ( 4.163799117101000559E-15, 0.000000000000000000, 34.00000000000000000 ) ) ;
#7197 = CARTESIAN_POINT ( 'NONE',  ( 5.425003271131650706, 0.000000000000000000, 0.000000000000000000 ) ) ;
#7198 = ORIENTED_EDGE ( 'NONE', *, *, #4882, .F. ) ;
#7199 = DIRECTION ( 'NONE',  ( 1.000000000000000000, 0.000000000000000000, 0.000000000000000000 ) ) ;
#7200 = ORIENTED_EDGE ( 'NONE', *, *, #596, .T. ) ;
#7201 = ADVANCED_FACE ( 'NONE', ( #1032 ), #989, .F. ) ;
#7202 = ORIENTED_EDGE ( 'NONE', *, *, #13682, .T. ) ;
#7203 = AXIS2_PLACEMENT_3D ( 'NONE', #8265, #6795, #10850 ) ;
#7204 = EDGE_CURVE ( 'NONE', #6787, #5898, #11834, .T. ) ;
#7205 = PLANE ( 'NONE',  #16306 ) ;
#7206 = EDGE_CURVE ( 'NONE', #15036, #3627, #10585, .T. ) ;
#7207 = SHAPE_DEFINITION_REPRESENTATION ( #6142, #7583 ) ;
#7208 = CIRCLE ( 'NONE', #6375, 13.69540538389601991 ) ;
#7209 = AXIS2_PLACEMENT_3D ( 'NONE', #10954, #10783, #16019 ) ;
#7210 =( NAMED_UNIT ( * ) PLANE_ANGLE_UNIT ( ) SI_UNIT ( $, .RADIAN. ) );
#7211 = AXIS2_PLACEMENT_3D ( 'NONE', #10421, #12911, #7746 ) ;
#7212 = AXIS2_PLACEMENT_3D ( 'NONE', #4934, #14052, #7760 ) ;
#7213 = LINE ( 'NONE', #16410, #5464 ) ;
#7214 = ORIENTED_EDGE ( 'NONE', *, *, #4440, .T. ) ;
#7215 = CARTESIAN_POINT ( 'NONE',  ( -39.99999999999997868, 0.000000000000000000, 26.00000000000000355 ) ) ;
#7216 = DIRECTION ( 'NONE',  ( -1.000000000000000000, -0.000000000000000000, -0.000000000000000000 ) ) ;
#7217 = VECTOR ( 'NONE', #6778, 1000.000000000000000 ) ;
#7218 = ORIENTED_EDGE ( 'NONE', *, *, #476, .F. ) ;
#7219 = DIRECTION ( 'NONE',  ( 0.000000000000000000, 1.224646799147356165E-16, 1.000000000000000000 ) ) ;
#7220 = DIRECTION ( 'NONE',  ( 0.000000000000000000, -0.3420201433256626067, -0.9396926207859105373 ) ) ;
#7221 = EDGE_LOOP ( 'NONE', ( #9550, #474, #3331, #803 ) ) ;
#7222 = AXIS2_PLACEMENT_3D ( 'NONE', #6346, #2590, #11772 ) ;
#7223 = DIRECTION ( 'NONE',  ( 1.000000000000000000, 0.000000000000000000, 0.000000000000000000 ) ) ;
#7224 = VECTOR ( 'NONE', #10337, 1000.000000000000000 ) ;
#7225 = ORIENTED_EDGE ( 'NONE', *, *, #3012, .T. ) ;
#7226 = ORIENTED_EDGE ( 'NONE', *, *, #15374, .F. ) ;
#7227 = AXIS2_PLACEMENT_3D ( 'NONE', #11910, #14666, #10532 ) ;
#7228 = ORIENTED_EDGE ( 'NONE', *, *, #12914, .F. ) ;
#7229 =( NAMED_UNIT ( * ) SI_UNIT ( $, .STERADIAN. ) SOLID_ANGLE_UNIT ( ) );
#7230 = AXIS2_PLACEMENT_3D ( 'NONE', #5833, #11081, #5921 ) ;
#7231 = ORIENTED_EDGE ( 'NONE', *, *, #3543, .F. ) ;
#7232 = ORIENTED_EDGE ( 'NONE', *, *, #4446, .F. ) ;
#7233 = DIRECTION ( 'NONE',  ( 0.000000000000000000, -1.000000000000000000, 0.000000000000000000 ) ) ;
#7234 = VECTOR ( 'NONE', #11682, 1000.000000000000000 ) ;
#7235 = PLANE ( 'NONE',  #10729 ) ;
#7236 = CARTESIAN_POINT ( 'NONE',  ( 31.00000000000003553, 19.00000000000000000, 20.99999999999999289 ) ) ;
#7237 = DIRECTION ( 'NONE',  ( 0.000000000000000000, -1.000000000000000000, 0.000000000000000000 ) ) ;
#7238 = VECTOR ( 'NONE', #15707, 1000.000000000000227 ) ;
#7239 = FACE_OUTER_BOUND ( 'NONE', #2929, .T. ) ;
#7240 = CARTESIAN_POINT ( 'NONE',  ( 31.81980515339464333, 11.00000000000000000, -35.11980515339463693 ) ) ;
#7241 = DIRECTION ( 'NONE',  ( 0.000000000000000000, 0.000000000000000000, -1.000000000000000000 ) ) ;
#7242 = DIRECTION ( 'NONE',  ( 0.000000000000000000, 0.000000000000000000, 1.000000000000000000 ) ) ;
#7243 = VERTEX_POINT ( 'NONE', #2470 ) ;
#7244 = FACE_OUTER_BOUND ( 'NONE', #16452, .T. ) ;
#7245 = CARTESIAN_POINT ( 'NONE',  ( -55.99999999999988631, 173.0499717945046996, 146.7982946275220968 ) ) ;
#7246 = DIRECTION ( 'NONE',  ( 0.000000000000000000, 0.000000000000000000, -1.000000000000000000 ) ) ;
#7247 = VECTOR ( 'NONE', #4683, 1000.000000000000000 ) ;
#7248 = FACE_OUTER_BOUND ( 'NONE', #13969, .T. ) ;
#7250 = VERTEX_POINT ( 'NONE', #7789 ) ;
#7249 = EDGE_LOOP ( 'NONE', ( #4095, #4577 ) ) ;
#7251 = DIRECTION ( 'NONE',  ( 1.000000000000000000, 0.000000000000000000, 0.000000000000000000 ) ) ;
#7252 = AXIS2_PLACEMENT_3D ( 'NONE', #8322, #13656, #6066 ) ;
#7253 = VECTOR ( 'NONE', #9613, 1000.000000000000000 ) ;
#7254 = DIRECTION ( 'NONE',  ( 1.000000000000000000, 0.000000000000000000, 0.000000000000000000 ) ) ;
#7255 = EDGE_CURVE ( 'NONE', #1496, #13088, #4959, .T. ) ;
#7256 = PLANE ( 'NONE',  #3869 ) ;
#7257 = DIRECTION ( 'NONE',  ( 0.000000000000000000, -1.000000000000000000, 0.000000000000000000 ) ) ;
#7258 = ORIENTED_EDGE ( 'NONE', *, *, #4859, .T. ) ;
#7259 = CARTESIAN_POINT ( 'NONE',  ( 0.000000000000000000, 341.0487089519837696, -115.0000000000032969 ) ) ;
#7260 = LINE ( 'NONE', #16063, #688 ) ;
#7261 = ADVANCED_FACE ( 'NONE', ( #7877 ), #11753, .F. ) ;
#7262 = DIRECTION ( 'NONE',  ( -0.000000000000000000, -1.000000000000000000, -0.000000000000000000 ) ) ;
#7263 = ORIENTED_EDGE ( 'NONE', *, *, #5204, .F. ) ;
#7264 = CARTESIAN_POINT ( 'NONE',  ( 1.399999999999999911, 0.000000000000000000, 0.000000000000000000 ) ) ;
#7265 = AXIS2_PLACEMENT_3D ( 'NONE', #3746, #6212, #10181 ) ;
#7266 = CARTESIAN_POINT ( 'NONE',  ( -55.99999999999989342, 523.2161522479888163, -507.5890438806159750 ) ) ;
#7267 = DIRECTION ( 'NONE',  ( -1.000000000000000000, -0.000000000000000000, -0.000000000000000000 ) ) ;
#7268 = DIRECTION ( 'NONE',  ( 0.000000000000000000, 1.000000000000000000, 0.000000000000000000 ) ) ;
#7269 = FACE_OUTER_BOUND ( 'NONE', #6525, .T. ) ;
#7270 = EDGE_LOOP ( 'NONE', ( #14389, #7319, #8894, #14473 ) ) ;
#7271 = DIRECTION ( 'NONE',  ( 0.000000000000000000, 1.000000000000000000, 0.000000000000000000 ) ) ;
#7272 = CONICAL_SURFACE ( 'NONE', #13370, 18.17500000000000071, 0.7483780475235185525 ) ;
#7273 = LINE ( 'NONE', #11316, #7930 ) ;
#7274 = EDGE_CURVE ( 'NONE', #13076, #8177, #14984, .T. ) ;
#7275 = AXIS2_PLACEMENT_3D ( 'NONE', #4045, #442, #1555 ) ;
#7276 = VERTEX_POINT ( 'NONE', #5049 ) ;
#7277 = ADVANCED_FACE ( 'NONE', ( #14419 ), #9780, .F. ) ;
#7278 = DIRECTION ( 'NONE',  ( -0.000000000000000000, 0.000000000000000000, 1.000000000000000000 ) ) ;
#7279 = ORIENTED_EDGE ( 'NONE', *, *, #12252, .T. ) ;
#7280 = CARTESIAN_POINT ( 'NONE',  ( -430.0000000000000568, 620.7506394335853201, 109.9999999999999858 ) ) ;
#7281 = ADVANCED_FACE ( 'NONE', ( #7698 ), #15618, .T. ) ;
#7282 = EDGE_CURVE ( 'NONE', #11595, #3880, #1537, .T. ) ;
#7283 = DIRECTION ( 'NONE',  ( 0.000000000000000000, 0.000000000000000000, 1.000000000000000000 ) ) ;
#7284 = ORIENTED_EDGE ( 'NONE', *, *, #15167, .F. ) ;
#7285 = PLANE ( 'NONE',  #12195 ) ;
#7286 = EDGE_CURVE ( 'NONE', #11419, #8068, #10635, .T. ) ;
#7287 = DIRECTION ( 'NONE',  ( 0.000000000000000000, -7.137148015447440312E-15, 1.000000000000000000 ) ) ;
#7288 = FACE_OUTER_BOUND ( 'NONE', #12143, .T. ) ;
#7289 = VERTEX_POINT ( 'NONE', #2729 ) ;
#7290 = VECTOR ( 'NONE', #4804, 1000.000000000000000 ) ;
#7291 = AXIS2_PLACEMENT_3D ( 'NONE', #4626, #16474, #10046 ) ;
#7292 = SURFACE_STYLE_FILL_AREA ( #8431 ) ;
#7293 = PLANE ( 'NONE',  #8447 ) ;
#7294 = ORIENTED_EDGE ( 'NONE', *, *, #167, .F. ) ;
#7295 = ORIENTED_EDGE ( 'NONE', *, *, #6418, .T. ) ;
#7296 = CARTESIAN_POINT ( 'NONE',  ( 29.68009836720079875, 352.3758082234937206, -75.00000000000000000 ) ) ;
#7297 = SHAPE_DEFINITION_REPRESENTATION ( #10980, #5843 ) ;
#7298 = EDGE_CURVE ( 'NONE', #15837, #4299, #472, .T. ) ;
#7299 = LINE ( 'NONE', #12549, #7377 ) ;
#7300 = AXIS2_PLACEMENT_3D ( 'NONE', #8573, #10032, #2202 ) ;
#7301 = ORIENTED_EDGE ( 'NONE', *, *, #193, .F. ) ;
#7302 = AXIS2_PLACEMENT_3D ( 'NONE', #4611, #1871, #11058 ) ;
#7303 = DIRECTION ( 'NONE',  ( 1.000000000000000000, 0.000000000000000000, 0.000000000000000000 ) ) ;
#7304 = EDGE_CURVE ( 'NONE', #175, #6882, #3079, .T. ) ;
#7305 = CYLINDRICAL_SURFACE ( 'NONE', #11911, 10.00000000000000178 ) ;
#7306 = EDGE_CURVE ( 'NONE', #10664, #7586, #8145, .T. ) ;
#7307 = ORIENTED_EDGE ( 'NONE', *, *, #16539, .F. ) ;
#7308 = LINE ( 'NONE', #5857, #3952 ) ;
#7309 = EDGE_CURVE ( 'NONE', #7606, #8690, #5734, .T. ) ;
#7310 = DIRECTION ( 'NONE',  ( -0.000000000000000000, -1.000000000000000000, -0.000000000000000000 ) ) ;
#7311 = ORIENTED_EDGE ( 'NONE', *, *, #5931, .T. ) ;
#7312 = LINE ( 'NONE', #8525, #4497 ) ;
#7313 = VERTEX_POINT ( 'NONE', #5654 ) ;
#7314 = ORIENTED_EDGE ( 'NONE', *, *, #7160, .F. ) ;
#7315 = TOROIDAL_SURFACE ( 'NONE', #1016, 4.695405383895982609, 9.000000000000000000 ) ;
#7316 = AXIS2_PLACEMENT_3D ( 'NONE', #6797, #16254, #12054 ) ;
#7317 = ORIENTED_EDGE ( 'NONE', *, *, #4153, .F. ) ;
#7318 = EDGE_CURVE ( 'NONE', #2563, #199, #9517, .T. ) ;
#7319 = ORIENTED_EDGE ( 'NONE', *, *, #13904, .F. ) ;
#7320 = ORIENTED_EDGE ( 'NONE', *, *, #5284, .T. ) ;
#7321 = DIRECTION ( 'NONE',  ( 0.000000000000000000, 0.000000000000000000, -1.000000000000000000 ) ) ;
#7322 = DIRECTION ( 'NONE',  ( 0.000000000000000000, 0.000000000000000000, -1.000000000000000000 ) ) ;
#7323 = CARTESIAN_POINT ( 'NONE',  ( 37.00000000000000000, 0.000000000000000000, 23.00000000000001066 ) ) ;
#7324 = COLOUR_RGB ( '', 0.31764706, 0.68627451, 0.89019608) ;
#7325 = FACE_OUTER_BOUND ( 'NONE', #5516, .T. ) ;
#7326 = DIRECTION ( 'NONE',  ( 1.000000000000000000, 0.000000000000000000, -0.000000000000000000 ) ) ;
#7327 = PLANE ( 'NONE',  #643 ) ;
#7328 = CARTESIAN_POINT ( 'NONE',  ( 0.000000000000000000, 50.00000000000000000, 0.000000000000000000 ) ) ;
#7329 = DIRECTION ( 'NONE',  ( -0.000000000000000000, 1.000000000000000000, -0.000000000000000000 ) ) ;
#7330 = VERTEX_POINT ( 'NONE', #10810 ) ;
#7331 = DIRECTION ( 'NONE',  ( -0.000000000000000000, -1.000000000000000000, -0.000000000000000000 ) ) ;
#7332 = LINE ( 'NONE', #15330, #12421 ) ;
#7333 = FACE_OUTER_BOUND ( 'NONE', #6230, .T. ) ;
#7335 = ORIENTED_EDGE ( 'NONE', *, *, #13997, .F. ) ;
#7334 = ORIENTED_EDGE ( 'NONE', *, *, #4793, .F. ) ;
#7336 = AXIS2_PLACEMENT_3D ( 'NONE', #930, #8823, #7177 ) ;
#7337 = CARTESIAN_POINT ( 'NONE',  ( 1.163414460601643398E-15, 38.00000000000000711, 9.500000000000000000 ) ) ;
#7338 = EDGE_CURVE ( 'NONE', #13962, #9616, #6468, .T. ) ;
#7339 = CARTESIAN_POINT ( 'NONE',  ( -46.99999999999988631, 493.2350855268092573, -589.9613477082210693 ) ) ;
#7340 = CARTESIAN_POINT ( 'NONE',  ( 27.49999999999999645, 196.3050121726289206, 0.000000000000000000 ) ) ;
#7341 = VERTEX_POINT ( 'NONE', #15952 ) ;
#7342 = EDGE_CURVE ( 'NONE', #16466, #5917, #9244, .T. ) ;
#7343 = DIRECTION ( 'NONE',  ( 0.000000000000000000, 0.000000000000000000, -1.000000000000000000 ) ) ;
#7344 = FACE_OUTER_BOUND ( 'NONE', #4462, .T. ) ;
#7345 = ORIENTED_EDGE ( 'NONE', *, *, #13170, .F. ) ;
#7346 = DIRECTION ( 'NONE',  ( -1.000000000000000000, 0.000000000000000000, 0.000000000000000000 ) ) ;
#7347 = AXIS2_PLACEMENT_3D ( 'NONE', #6780, #2664, #10653 ) ;
#7348 = CARTESIAN_POINT ( 'NONE',  ( 1.231978928595278688E-12, 193.4898140233672450, 37.52989836422093362 ) ) ;
#7349 = DIRECTION ( 'NONE',  ( 0.000000000000000000, -1.000000000000000000, 0.000000000000000000 ) ) ;
#7350 = PRODUCT_DEFINITION ( 'UNKNOWN', '', #8910, #4860 ) ;
#7351 = CARTESIAN_POINT ( 'NONE',  ( 3.000000000000000000, 6.000000000000000000, 22.00000000000000000 ) ) ;
#7352 = DIRECTION ( 'NONE',  ( 0.7327934916262990317, -0.6804510993672779895, 8.333122608164345406E-17 ) ) ;
#7353 = ORIENTED_EDGE ( 'NONE', *, *, #7338, .F. ) ;
#7354 = CARTESIAN_POINT ( 'NONE',  ( 0.7366000000000293424, 218.4499468633031825, 287.1312267635914850 ) ) ;
#7355 = EDGE_CURVE ( 'NONE', #2950, #6153, #4309, .T. ) ;
#7356 = DIRECTION ( 'NONE',  ( 0.000000000000000000, -0.6427876096865372535, 0.7660444431189797898 ) ) ;
#7357 = ORIENTED_EDGE ( 'NONE', *, *, #16414, .T. ) ;
#7358 = VECTOR ( 'NONE', #3154, 1000.000000000000000 ) ;
#7359 = ORIENTED_EDGE ( 'NONE', *, *, #15291, .T. ) ;
#7360 = DIRECTION ( 'NONE',  ( 0.000000000000000000, 0.000000000000000000, -1.000000000000000000 ) ) ;
#7361 = LINE ( 'NONE', #3265, #13887 ) ;
#7362 = ORIENTED_EDGE ( 'NONE', *, *, #4062, .F. ) ;
#7363 = FACE_OUTER_BOUND ( 'NONE', #9368, .T. ) ;
#7364 = DIRECTION ( 'NONE',  ( 1.000000000000000000, -0.000000000000000000, 0.000000000000000000 ) ) ;
#7365 = DIRECTION ( 'NONE',  ( 0.000000000000000000, 0.000000000000000000, -1.000000000000000000 ) ) ;
#7366 = ORIENTED_EDGE ( 'NONE', *, *, #12331, .T. ) ;
#7367 = ADVANCED_FACE ( 'NONE', ( #16133 ), #16049, .F. ) ;
#7368 = PRODUCT_DEFINITION_SHAPE ( 'NONE', 'NONE',  #10407 ) ;
#7369 = DIRECTION ( 'NONE',  ( 0.000000000000000000, 0.000000000000000000, 1.000000000000000000 ) ) ;
#7370 = CARTESIAN_POINT ( 'NONE',  ( 10.00000000000000000, 372.8685141053783241, -146.8198051533979935 ) ) ;
#7371 = CARTESIAN_POINT ( 'NONE',  ( -3.269999999999640750, 285.9618298588721927, 37.54886172132344768 ) ) ;
#7372 = EDGE_LOOP ( 'NONE', ( #8978, #6181, #11548, #7992 ) ) ;
#7373 = ORIENTED_EDGE ( 'NONE', *, *, #2555, .T. ) ;
#7374 = CYLINDRICAL_SURFACE ( 'NONE', #10004, 13.69540538389601991 ) ;
#7375 = APPLICATION_PROTOCOL_DEFINITION ( 'draft international standard', 'automotive_design', 1998, #4131 ) ;
#7376 = EDGE_CURVE ( 'NONE', #13527, #16649, #2992, .T. ) ;
#7377 = VECTOR ( 'NONE', #792, 1000.000000000000000 ) ;
#7378 = CARTESIAN_POINT ( 'NONE',  ( 2.383085342081995517, 61.83271933867543169, 9.196931476227284463 ) ) ;
#7379 = VERTEX_POINT ( 'NONE', #9529 ) ;
#7380 = DIRECTION ( 'NONE',  ( 1.000000000000000000, -0.000000000000000000, 0.000000000000000000 ) ) ;
#7381 = CYLINDRICAL_SURFACE ( 'NONE', #13015, 2.999999999999999112 ) ;
#7382 = ORIENTED_EDGE ( 'NONE', *, *, #10974, .F. ) ;
#7383 = DIRECTION ( 'NONE',  ( 3.474153781073083121E-15, -1.000000000000000000, 0.000000000000000000 ) ) ;
#7384 = CARTESIAN_POINT ( 'NONE',  ( -22.99999999999999645, 68.00000000000000000, 37.00000000000002132 ) ) ;
#7385 = VERTEX_POINT ( 'NONE', #9440 ) ;
#7386 = AXIS2_PLACEMENT_3D ( 'NONE', #2714, #2540, #12855 ) ;
#7387 = ADVANCED_FACE ( 'NONE', ( #8056 ), #3478, .T. ) ;
#7388 = DIRECTION ( 'NONE',  ( -0.000000000000000000, 1.000000000000000000, -0.000000000000000000 ) ) ;
#7389 = VERTEX_POINT ( 'NONE', #12190 ) ;
#7390 = ORIENTED_EDGE ( 'NONE', *, *, #8083, .F. ) ;
#7391 = ORIENTED_EDGE ( 'NONE', *, *, #5235, .T. ) ;
#7392 = EDGE_CURVE ( 'NONE', #4190, #3286, #8312, .T. ) ;
#7393 = EDGE_CURVE ( 'NONE', #7039, #14972, #1447, .T. ) ;
#7394 = EDGE_CURVE ( 'NONE', #16255, #12090, #6676, .T. ) ;
#7395 = ADVANCED_FACE ( 'NONE', ( #12014 ), #9348, .F. ) ;
#7396 = VERTEX_POINT ( 'NONE', #4782 ) ;
#7397 = AXIS2_PLACEMENT_3D ( 'NONE', #6887, #14638, #2868 ) ;
#7398 = EDGE_LOOP ( 'NONE', ( #16889, #14841, #3494, #11524 ) ) ;
#7399 = DIRECTION ( 'NONE',  ( 0.000000000000000000, 0.000000000000000000, -1.000000000000000000 ) ) ;
#7400 = AXIS2_PLACEMENT_3D ( 'NONE', #12094, #9606, #9528 ) ;
#7401 = LINE ( 'NONE', #813, #12924 ) ;
#7402 = DIRECTION ( 'NONE',  ( 0.000000000000000000, -1.000000000000000000, -1.321694076934710402E-16 ) ) ;
#7403 = APPLICATION_CONTEXT ( 'automotive_design' ) ;
#7404 = DIRECTION ( 'NONE',  ( -0.000000000000000000, -1.000000000000000000, -0.000000000000000000 ) ) ;
#7405 = DIRECTION ( 'NONE',  ( -1.196361017915039486E-16, -0.000000000000000000, -1.000000000000000000 ) ) ;
#7406 = DIRECTION ( 'NONE',  ( 0.000000000000000000, 0.000000000000000000, 1.000000000000000000 ) ) ;
#7407 = CARTESIAN_POINT ( 'NONE',  ( 18.99999999999998224, 8.000000000000000000, -39.99999999999999289 ) ) ;
#7408 = VERTEX_POINT ( 'NONE', #5815 ) ;
#7409 = DIRECTION ( 'NONE',  ( -0.000000000000000000, -1.000000000000000000, -0.000000000000000000 ) ) ;
#7410 = CARTESIAN_POINT ( 'NONE',  ( -32.00000000000000711, 6.000000000000000000, -22.00000000000000355 ) ) ;
#7411 = CIRCLE ( 'NONE', #2208, 4.999999999999997335 ) ;
#7412 = CARTESIAN_POINT ( 'NONE',  ( 39.41161623800082481, 323.9612906317821057, -6.736600000000000144 ) ) ;
#7414 = VERTEX_POINT ( 'NONE', #590 ) ;
#7413 = ORIENTED_EDGE ( 'NONE', *, *, #16143, .F. ) ;
#7415 = PLANE ( 'NONE',  #13875 ) ;
#7416 = ADVANCED_FACE ( 'NONE', ( #2035 ), #16304, .T. ) ;
#7417 = PLANE ( 'NONE',  #9382 ) ;
#7418 = CARTESIAN_POINT ( 'NONE',  ( 10.00000000000000000, 620.7506394335853201, 109.9999999999999858 ) ) ;
#7419 = DIRECTION ( 'NONE',  ( 0.000000000000000000, -0.000000000000000000, 1.000000000000000000 ) ) ;
#7420 = AXIS2_PLACEMENT_3D ( 'NONE', #7759, #13021, #9154 ) ;
#7421 = EDGE_LOOP ( 'NONE', ( #9748, #4534, #13217, #14171 ) ) ;
#7422 = PRODUCT_DEFINITION_CONTEXT ( 'detailed design', #2702, 'design' ) ;
#7423 = DIRECTION ( 'NONE',  ( 0.000000000000000000, 0.000000000000000000, -1.000000000000000000 ) ) ;
#7424 = DIRECTION ( 'NONE',  ( -1.000000000000000000, -0.000000000000000000, -0.000000000000000000 ) ) ;
#7425 = EDGE_LOOP ( 'NONE', ( #5757, #16403, #10944, #1008 ) ) ;
#7426 = DIRECTION ( 'NONE',  ( 0.000000000000000000, 0.000000000000000000, 1.000000000000000000 ) ) ;
#7427 = CARTESIAN_POINT ( 'NONE',  ( -1.281199806751509129, 189.9796977361249617, 37.61247111518789410 ) ) ;
#7428 = CARTESIAN_POINT ( 'NONE',  ( 35.99999999999999289, 10.00000000000000000, 18.99999999999999289 ) ) ;
#7429 = DIRECTION ( 'NONE',  ( -1.000000000000000000, 0.000000000000000000, 0.000000000000000000 ) ) ;
#7430 = LINE ( 'NONE', #5984, #2129 ) ;
#7431 = ORIENTED_EDGE ( 'NONE', *, *, #12150, .F. ) ;
#7432 = AXIS2_PLACEMENT_3D ( 'NONE', #7995, #12134, #1485 ) ;
#7433 = PLANE ( 'NONE',  #16855 ) ;
#7434 = CARTESIAN_POINT ( 'NONE',  ( 31.00000000000001421, 0.000000000000000000, 22.99999999999999645 ) ) ;
#7435 = CLOSED_SHELL ( 'NONE', ( #13816, #4382, #8463, #2383, #16257, #12121, #5310, #11057, #16192, #4574, #8533, #8373, #4381, #10119, #10147, #8376, #4701, #7696, #2896, #6160, #14492, #8866, #14652, #4362, #8497, #14714, #10364, #8767, #11808, #14046, #2168, #3636, #3789, #10423, #12553, #12319, #4644, #13692, #7395, #1125, #8990, #1409, #7281, #1609, #13937, #2582, #1874, #15060, #5493, #2171, #15683, #7551, #6317, #2447, #6136, #9637, #12788, #13933, #6115, #12454, #16954, #4231, #10145, #11468, #13934, #10645, #4148, #3005, #2581, #9895, #8349, #13815, #3219, #5699, #990, #8466, #10029, #4636, #4971, #12359, #7387, #15395, #407, #5621, #3864, #441, #10945, #3973, #3712, #3521, #10345, #1577, #13767, #2795, #456, #4530, #3635, #10873, #5628, #13322, #9589, #15381, #1638, #12857, #7923, #7602, #4285, #14429, #618, #12973, #3537, #720, #14860, #9174 ) ) ;
#7436 = AXIS2_PLACEMENT_3D ( 'NONE', #2547, #6235, #12941 ) ;
#7437 = DIRECTION ( 'NONE',  ( -1.000000000000000000, 0.000000000000000000, -0.000000000000000000 ) ) ;
#7438 = ORIENTED_EDGE ( 'NONE', *, *, #5727, .T. ) ;
#7439 = FACE_OUTER_BOUND ( 'NONE', #1029, .T. ) ;
#7440 = CIRCLE ( 'NONE', #5246, 13.69540538389601991 ) ;
#7441 = DIRECTION ( 'NONE',  ( -1.000000000000000000, -0.000000000000000000, -0.000000000000000000 ) ) ;
#7442 = EDGE_LOOP ( 'NONE', ( #4344, #6864, #14932, #11871 ) ) ;
#7443 = DIRECTION ( 'NONE',  ( 1.000000000000000000, -0.000000000000000000, -0.000000000000000000 ) ) ;
#7444 = LINE ( 'NONE', #13917, #10656 ) ;
#7445 = CYLINDRICAL_SURFACE ( 'NONE', #5925, 15.00000000000000000 ) ;
#7446 = ORIENTED_EDGE ( 'NONE', *, *, #3086, .T. ) ;
#7447 = AXIS2_PLACEMENT_3D ( 'NONE', #13402, #1621, #14769 ) ;
#7448 = AXIS2_PLACEMENT_3D ( 'NONE', #11996, #406, #1779 ) ;
#7449 = DIRECTION ( 'NONE',  ( 0.000000000000000000, 1.000000000000000000, 0.000000000000000000 ) ) ;
#7450 = VECTOR ( 'NONE', #9909, 1000.000000000000000 ) ;
#7451 = CARTESIAN_POINT ( 'NONE',  ( 31.99999999999998579, 6.000000000000000000, 25.99999999999999645 ) ) ;
#7452 = DIRECTION ( 'NONE',  ( 0.000000000000000000, -0.9271838545667883125, -0.3746065934159094613 ) ) ;
#7453 = ORIENTED_EDGE ( 'NONE', *, *, #9315, .T. ) ;
#7454 = PRODUCT_CONTEXT ( 'NONE', #3036, 'mechanical' ) ;
#7455 = DIRECTION ( 'NONE',  ( 1.000000000000000000, 0.000000000000000000, 0.000000000000000000 ) ) ;
#7456 = ORIENTED_EDGE ( 'NONE', *, *, #1483, .F. ) ;
#7457 = EDGE_CURVE ( 'NONE', #2891, #9064, #4540, .T. ) ;
#7458 = AXIS2_PLACEMENT_3D ( 'NONE', #12413, #14911, #5884 ) ;
#7459 = CIRCLE ( 'NONE', #13797, 2.500000000000002220 ) ;
#7460 = CARTESIAN_POINT ( 'NONE',  ( 40.00000000000000711, 11.00000000000000000, 34.99999999999997868 ) ) ;
#7461 = LINE ( 'NONE', #16826, #6972 ) ;
#7462 = ORIENTED_EDGE ( 'NONE', *, *, #716, .T. ) ;
#7463 = CARTESIAN_POINT ( 'NONE',  ( 30.99999999999999645, 3.000000000000000000, 26.00000000000000355 ) ) ;
#7464 = CARTESIAN_POINT ( 'NONE',  ( -30.99999999999999289, 68.00000000000000000, 31.00000000000000000 ) ) ;
#7465 = ORIENTED_EDGE ( 'NONE', *, *, #4156, .F. ) ;
#7466 = AXIS2_PLACEMENT_3D ( 'NONE', #12576, #7326, #14842 ) ;
#7467 = EDGE_CURVE ( 'NONE', #49, #12012, #16897, .T. ) ;
#7468 = LINE ( 'NONE', #12734, #3129 ) ;
#7469 = VERTEX_POINT ( 'NONE', #8660 ) ;
#7470 = EDGE_LOOP ( 'NONE', ( #11714, #4832, #14191, #9292 ) ) ;
#7471 = AXIS2_PLACEMENT_3D ( 'NONE', #8189, #13443, #5612 ) ;
#7472 = AXIS2_PLACEMENT_3D ( 'NONE', #502, #1869, #13884 ) ;
#7473 = ORIENTED_EDGE ( 'NONE', *, *, #5632, .F. ) ;
#7474 = VERTEX_POINT ( 'NONE', #7266 ) ;
#7475 = AXIS2_PLACEMENT_3D ( 'NONE', #3620, #8701, #13759 ) ;
#7476 = ORIENTED_EDGE ( 'NONE', *, *, #9827, .T. ) ;
#7477 = EDGE_CURVE ( 'NONE', #6600, #14523, #5377, .T. ) ;
#7478 = DIRECTION ( 'NONE',  ( 1.000000000000000000, 0.000000000000000000, 0.000000000000000000 ) ) ;
#7479 = DIRECTION ( 'NONE',  ( 0.000000000000000000, 1.000000000000000000, 0.000000000000000000 ) ) ;
#7480 = CIRCLE ( 'NONE', #4762, 20.75209553982837463 ) ;
#7481 = VECTOR ( 'NONE', #15325, 1000.000000000000000 ) ;
#7482 = CARTESIAN_POINT ( 'NONE',  ( 4.163799117101000559E-15, 16.00000000000000000, 34.00000000000000000 ) ) ;
#7483 = CARTESIAN_POINT ( 'NONE',  ( -22.00000000000001776, 6.000000000000000000, 32.00000000000000711 ) ) ;
#7484 = AXIS2_PLACEMENT_3D ( 'NONE', #9404, #9243, #483 ) ;
#7485 = CARTESIAN_POINT ( 'NONE',  ( 3.850000000000000089, 0.000000000000000000, 0.000000000000000000 ) ) ;
#7486 = EDGE_CURVE ( 'NONE', #15703, #3270, #1876, .T. ) ;
#7487 = EDGE_CURVE ( 'NONE', #199, #2563, #15542, .T. ) ;
#7488 = DIRECTION ( 'NONE',  ( -1.000000000000000000, 0.000000000000000000, 0.000000000000000000 ) ) ;
#7489 = EDGE_CURVE ( 'NONE', #1719, #15142, #16462, .T. ) ;
#7490 = CIRCLE ( 'NONE', #114, 5.268482129199949959 ) ;
#7491 = LINE ( 'NONE', #8467, #9405 ) ;
#7492 = ORIENTED_EDGE ( 'NONE', *, *, #14479, .F. ) ;
#7493 = CARTESIAN_POINT ( 'NONE',  ( -31.00000000000000000, 19.00000000000000000, -31.00000000000000000 ) ) ;
#7494 = FACE_OUTER_BOUND ( 'NONE', #11145, .T. ) ;
#7496 = TOROIDAL_SURFACE ( 'NONE', #16817, 4.695405383895982609, 9.000000000000000000 ) ;
#7495 = ADVANCED_BREP_SHAPE_REPRESENTATION ( '', ( #14111, #1488 ), #13563 ) ;
#7497 = ORIENTED_EDGE ( 'NONE', *, *, #1087, .T. ) ;
#7498 = DIRECTION ( 'NONE',  ( 0.000000000000000000, -0.3746065934159049648, -0.9271838545667903109 ) ) ;
#7500 = VERTEX_POINT ( 'NONE', #763 ) ;
#7499 = ORIENTED_EDGE ( 'NONE', *, *, #16422, .F. ) ;
#7501 = DIRECTION ( 'NONE',  ( 0.000000000000000000, 1.000000000000000000, 0.000000000000000000 ) ) ;
#7502 = AXIS2_PLACEMENT_3D ( 'NONE', #3139, #12064, #6805 ) ;
#7503 = AXIS2_PLACEMENT_3D ( 'NONE', #13348, #5343, #15991 ) ;
#7504 = EDGE_LOOP ( 'NONE', ( #14793, #5006, #11113, #11625 ) ) ;
#7505 = AXIS2_PLACEMENT_3D ( 'NONE', #10061, #15299, #16579 ) ;
#7506 = DIRECTION ( 'NONE',  ( 0.000000000000000000, 0.000000000000000000, -1.000000000000000000 ) ) ;
#7507 = FACE_OUTER_BOUND ( 'NONE', #994, .T. ) ;
#7508 = ORIENTED_EDGE ( 'NONE', *, *, #90, .F. ) ;
#7509 = PRODUCT_DEFINITION_SHAPE ( 'NONE', 'NONE',  #7350 ) ;
#7510 = CARTESIAN_POINT ( 'NONE',  ( 21.99999999999998224, 10.00000000000000000, -35.99999999999999289 ) ) ;
#7511 = ADVANCED_FACE ( 'NONE', ( #5981 ), #2597, .F. ) ;
#7512 = EDGE_CURVE ( 'NONE', #10513, #6709, #14153, .T. ) ;
#7513 = AXIS2_PLACEMENT_3D ( 'NONE', #1304, #5236, #2334 ) ;
#7514 = LINE ( 'NONE', #12773, #14173 ) ;
#7515 = ORIENTED_EDGE ( 'NONE', *, *, #7029, .F. ) ;
#7516 = CARTESIAN_POINT ( 'NONE',  ( 56.72999999999999687, 189.4632308570086536, 37.52989836422099046 ) ) ;
#7517 = EDGE_CURVE ( 'NONE', #1839, #11059, #185, .T. ) ;
#7518 = CIRCLE ( 'NONE', #134, 13.69540538389601991 ) ;
#7519 = DIRECTION ( 'NONE',  ( 0.000000000000000000, -0.6468954956981580739, 0.7625786632508375629 ) ) ;
#7520 = DIRECTION ( 'NONE',  ( -0.000000000000000000, -1.000000000000000000, -0.000000000000000000 ) ) ;
#7521 = AXIS2_PLACEMENT_3D ( 'NONE', #3428, #848, #8666 ) ;
#7522 = FACE_OUTER_BOUND ( 'NONE', #3679, .T. ) ;
#7523 = DIRECTION ( 'NONE',  ( -1.000000000000000000, -0.000000000000000000, 0.000000000000000000 ) ) ;
#7524 = ORIENTED_EDGE ( 'NONE', *, *, #6462, .F. ) ;
#7525 = CARTESIAN_POINT ( 'NONE',  ( 0.000000000000000000, 66.00000000000000000, 0.000000000000000000 ) ) ;
#7526 = EDGE_CURVE ( 'NONE', #583, #49, #1010, .T. ) ;
#7527 = CARTESIAN_POINT ( 'NONE',  ( 9.796850830579020038E-16, 6.000000000000000000, 22.00000000000000000 ) ) ;
#7528 =( REPRESENTATION_RELATIONSHIP ('NONE','NONE', #15822, #12316 ) REPRESENTATION_RELATIONSHIP_WITH_TRANSFORMATION ( #5060 )SHAPE_REPRESENTATION_RELATIONSHIP( ) );
#7529 = DIRECTION ( 'NONE',  ( 1.000000000000000000, 0.000000000000000000, -7.709882115452498874E-16 ) ) ;
#7530 = ORIENTED_EDGE ( 'NONE', *, *, #4758, .T. ) ;
#7531 = VECTOR ( 'NONE', #11742, 1000.000000000000000 ) ;
#7532 = CARTESIAN_POINT ( 'NONE',  ( -34.99999999999998579, 0.000000000000000000, 21.00000000000000355 ) ) ;
#7533 = PLANE ( 'NONE',  #3204 ) ;
#7534 = ORIENTED_EDGE ( 'NONE', *, *, #12840, .T. ) ;
#7535 = DIRECTION ( 'NONE',  ( -3.407805566942604749E-15, -0.9950371902099890420, 0.09950371902099952592 ) ) ;
#7536 = CARTESIAN_POINT ( 'NONE',  ( 0.7365999999999666148, 289.4632308570086252, 37.52989836422091230 ) ) ;
#7537 = LINE ( 'NONE', #10463, #2634 ) ;
#7538 = ORIENTED_EDGE ( 'NONE', *, *, #6429, .T. ) ;
#7539 = CARTESIAN_POINT ( 'NONE',  ( 30.99999999999997513, 10.00000000000000000, 30.99999999999999645 ) ) ;
#7540 = DIRECTION ( 'NONE',  ( 0.000000000000000000, 0.000000000000000000, -1.000000000000000000 ) ) ;
#7541 = CARTESIAN_POINT ( 'NONE',  ( 56.73000000000001108, 286.2094592450221739, 37.20452120302226007 ) ) ;
#7542 = EDGE_LOOP ( 'NONE', ( #10762, #8838, #14102, #12418 ) ) ;
#7543 = LINE ( 'NONE', #3783, #5047 ) ;
#7544 = CIRCLE ( 'NONE', #151, 9.000000000000007105 ) ;
#7545 =( LENGTH_UNIT ( ) NAMED_UNIT ( * ) SI_UNIT ( .MILLI., .METRE. ) );
#7546 = EDGE_CURVE ( 'NONE', #6048, #3292, #9162, .T. ) ;
#7547 = ORIENTED_EDGE ( 'NONE', *, *, #8546, .T. ) ;
#7548 = CARTESIAN_POINT ( 'NONE',  ( -25.99999999999999645, 0.000000000000000000, -31.00000000000003197 ) ) ;
#7549 = CARTESIAN_POINT ( 'NONE',  ( 31.00000000000000000, 19.00000000000000000, 30.99999999999999289 ) ) ;
#7550 = CIRCLE ( 'NONE', #1545, 84.99999999999997158 ) ;
#7551 = ADVANCED_FACE ( 'NONE', ( #9071, #6475, #11475, #14307, #3672, #7856, #16708, #8820, #13113, #1340, #5025 ), #15429, .T. ) ;
#7552 = DIRECTION ( 'NONE',  ( 0.000000000000000000, 1.000000000000000000, 0.000000000000000000 ) ) ;
#7553 = ORIENTED_EDGE ( 'NONE', *, *, #4237, .F. ) ;
#7554 = VECTOR ( 'NONE', #133, 1000.000000000000000 ) ;
#7555 = DIRECTION ( 'NONE',  ( -1.000000000000000000, 0.000000000000000000, 0.000000000000000000 ) ) ;
#7556 = DIRECTION ( 'NONE',  ( -1.000000000000000000, -0.000000000000000000, -0.000000000000000000 ) ) ;
#7557 = ORIENTED_EDGE ( 'NONE', *, *, #12250, .F. ) ;
#7558 = CARTESIAN_POINT ( 'NONE',  ( -46.99999999999988631, 493.2350855268092573, -571.5705369404290650 ) ) ;
#7559 = ORIENTED_EDGE ( 'NONE', *, *, #13723, .T. ) ;
#7560 = ORIENTED_EDGE ( 'NONE', *, *, #15747, .F. ) ;
#7561 = CARTESIAN_POINT ( 'NONE',  ( 31.81980515339464333, 8.000000000000000000, 35.11980515339463693 ) ) ;
#7562 = EDGE_LOOP ( 'NONE', ( #15140, #12848, #7353, #11001 ) ) ;
#7563 = DIRECTION ( 'NONE',  ( 1.000000000000000222, 0.000000000000000000, -1.387778780781445676E-17 ) ) ;
#7564 = AXIS2_PLACEMENT_3D ( 'NONE', #5561, #427, #2910 ) ;
#7565 = AXIS2_PLACEMENT_3D ( 'NONE', #12790, #2304, #11749 ) ;
#7566 = ORIENTED_EDGE ( 'NONE', *, *, #11694, .F. ) ;
#7567 = EDGE_CURVE ( 'NONE', #8258, #14799, #2096, .T. ) ;
#7568 = ORIENTED_EDGE ( 'NONE', *, *, #786, .T. ) ;
#7569 = CARTESIAN_POINT ( 'NONE',  ( 31.99999999999998579, 6.000000000000000000, 22.99999999999999645 ) ) ;
#7570 = DIRECTION ( 'NONE',  ( 0.000000000000000000, 1.000000000000000000, 0.000000000000000000 ) ) ;
#7571 = DIRECTION ( 'NONE',  ( 0.000000000000000000, 0.000000000000000000, 1.000000000000000000 ) ) ;
#7572 = FACE_OUTER_BOUND ( 'NONE', #11190, .T. ) ;
#7573 = LINE ( 'NONE', #6448, #11909 ) ;
#7574 = CIRCLE ( 'NONE', #13368, 9.000000000000007105 ) ;
#7575 = DIRECTION ( 'NONE',  ( 0.000000000000000000, 0.000000000000000000, -1.000000000000000000 ) ) ;
#7576 = AXIS2_PLACEMENT_3D ( 'NONE', #9481, #294, #2949 ) ;
#7577 = CARTESIAN_POINT ( 'NONE',  ( 3.850000000000000089, 0.000000000000000000, 0.000000000000000000 ) ) ;
#7578 = ORIENTED_EDGE ( 'NONE', *, *, #404, .F. ) ;
#7579 = LINE ( 'NONE', #6366, #4578 ) ;
#7580 = DIRECTION ( 'NONE',  ( -0.000000000000000000, 0.000000000000000000, -1.000000000000000000 ) ) ;
#7581 = VERTEX_POINT ( 'NONE', #12852 ) ;
#7582 = ADVANCED_FACE ( 'NONE', ( #1084 ), #5114, .T. ) ;
#7583 = SHAPE_REPRESENTATION ( '722909', ( #1488 ), #5871 ) ;
#7584 = LINE ( 'NONE', #16941, #11525 ) ;
#7586 = VERTEX_POINT ( 'NONE', #2536 ) ;
#7585 = EDGE_LOOP ( 'NONE', ( #2018, #13763, #2467, #8936, #12058 ) ) ;
#7587 = CARTESIAN_POINT ( 'NONE',  ( 25.99999999999998224, 0.000000000000000000, -31.00000000000003197 ) ) ;
#7588 = ORIENTED_EDGE ( 'NONE', *, *, #13617, .T. ) ;
#7589 = AXIS2_PLACEMENT_3D ( 'NONE', #9189, #4377, #9533 ) ;
#7590 = EDGE_CURVE ( 'NONE', #2493, #3786, #1257, .T. ) ;
#7591 = DIRECTION ( 'NONE',  ( 0.000000000000000000, -1.000000000000000000, 0.000000000000000000 ) ) ;
#7592 = DIRECTION ( 'NONE',  ( 0.000000000000000000, -0.9950371902099879318, -0.09950371902101125265 ) ) ;
#7593 = DIRECTION ( 'NONE',  ( 1.000000000000000000, 0.000000000000000000, 0.000000000000000000 ) ) ;
#7594 = VERTEX_POINT ( 'NONE', #5187 ) ;
#7595 = UNCERTAINTY_MEASURE_WITH_UNIT (LENGTH_MEASURE( 1.000000000000000082E-05 ), #11678, 'distance_accuracy_value', 'NONE');
#7596 = DIRECTION ( 'NONE',  ( -1.000000000000000000, 0.000000000000000000, 0.000000000000000000 ) ) ;
#7597 = ORIENTED_EDGE ( 'NONE', *, *, #2867, .T. ) ;
#7598 = DIRECTION ( 'NONE',  ( 1.000000000000000000, 0.000000000000000000, 0.000000000000000000 ) ) ;
#7599 = DIRECTION ( 'NONE',  ( 0.000000000000000000, 0.000000000000000000, 1.000000000000000000 ) ) ;
#7600 = PLANE ( 'NONE',  #9678 ) ;
#7601 =( GEOMETRIC_REPRESENTATION_CONTEXT ( 3 ) GLOBAL_UNCERTAINTY_ASSIGNED_CONTEXT ( ( #3667 ) ) GLOBAL_UNIT_ASSIGNED_CONTEXT ( ( #15870, #10982, #5472 ) ) REPRESENTATION_CONTEXT ( 'NONE', 'WORKASPACE' ) );
#7602 = ADVANCED_FACE ( 'NONE', ( #10440 ), #738, .T. ) ;
#7603 = FACE_OUTER_BOUND ( 'NONE', #7421, .T. ) ;
#7604 = EDGE_CURVE ( 'NONE', #10097, #14532, #14229, .T. ) ;
#7605 = FACE_BOUND ( 'NONE', #14455, .T. ) ;
#7606 = VERTEX_POINT ( 'NONE', #8996 ) ;
#7607 = CARTESIAN_POINT ( 'NONE',  ( -55.99999999999988631, 460.1944820612779381, -191.6957561970704660 ) ) ;
#7608 = EDGE_CURVE ( 'NONE', #15367, #10898, #12932, .T. ) ;
#7609 = ADVANCED_FACE ( 'NONE', ( #14400 ), #16878, .F. ) ;
#7610 = EDGE_CURVE ( 'NONE', #10013, #7981, #1279, .T. ) ;
#7611 = LINE ( 'NONE', #7778, #7709 ) ;
#7612 = EDGE_CURVE ( 'NONE', #9484, #8747, #16027, .T. ) ;
#7613 = CARTESIAN_POINT ( 'NONE',  ( 0.000000000000000000, 185.0000000000000568, -1.831360450120427585E-14 ) ) ;
#7614 = ORIENTED_EDGE ( 'NONE', *, *, #10552, .F. ) ;
#7615 = VECTOR ( 'NONE', #8334, 1000.000000000000000 ) ;
#7616 = DIRECTION ( 'NONE',  ( 0.000000000000000000, 1.000000000000000000, 0.000000000000000000 ) ) ;
#7617 = CARTESIAN_POINT ( 'NONE',  ( 3.850000000000000089, 1.778491767751089605E-15, 14.27500000000000036 ) ) ;
#7618 = EDGE_LOOP ( 'NONE', ( #13271, #3547, #8865, #6454 ) ) ;
#7619 = DIRECTION ( 'NONE',  ( -0.000000000000000000, -0.000000000000000000, 1.000000000000000000 ) ) ;
#7620 = DIRECTION ( 'NONE',  ( 0.000000000000000000, 0.000000000000000000, 1.000000000000000000 ) ) ;
#7621 = FACE_OUTER_BOUND ( 'NONE', #7922, .T. ) ;
#7622 = EDGE_LOOP ( 'NONE', ( #11893, #2491, #9308, #8780 ) ) ;
#7623 =( LENGTH_UNIT ( ) NAMED_UNIT ( * ) SI_UNIT ( .MILLI., .METRE. ) );
#7624 = PLANE ( 'NONE',  #3772 ) ;
#7625 = DIRECTION ( 'NONE',  ( 0.000000000000000000, 0.000000000000000000, -1.000000000000000000 ) ) ;
#7626 = VERTEX_POINT ( 'NONE', #9587 ) ;
#7627 = PLANE ( 'NONE',  #1795 ) ;
#7628 = AXIS2_PLACEMENT_3D ( 'NONE', #5996, #3101, #6407 ) ;
#7629 = ITEM_DEFINED_TRANSFORMATION ( 'NONE', 'NONE', #12474,  #1488 ) ;
#7630 = APPLICATION_CONTEXT ( 'automotive_design' ) ;
#7631 = ADVANCED_FACE ( 'NONE', ( #14827 ), #1426, .F. ) ;
#7632 = EDGE_LOOP ( 'NONE', ( #16848, #3995, #4220, #1184, #12968 ) ) ;
#7633 = DIRECTION ( 'NONE',  ( 0.000000000000000000, 0.000000000000000000, -1.000000000000000000 ) ) ;
#7634 = DIRECTION ( 'NONE',  ( -1.000000000000000000, -0.000000000000000000, -0.000000000000000000 ) ) ;
#7635 = LINE ( 'NONE', #5066, #1670 ) ;
#7636 = EDGE_LOOP ( 'NONE', ( #15196, #9084 ) ) ;
#7637 = LINE ( 'NONE', #12889, #11890 ) ;
#7638 = CARTESIAN_POINT ( 'NONE',  ( 2.799999999999999822, 13.30000000000000071, 0.000000000000000000 ) ) ;
#7639 = ORIENTED_EDGE ( 'NONE', *, *, #7204, .F. ) ;
#7640 = CARTESIAN_POINT ( 'NONE',  ( 37.00000000000000000, 0.000000000000000000, 23.00000000000001066 ) ) ;
#7641 = EDGE_CURVE ( 'NONE', #5615, #15480, #5669, .T. ) ;
#7642 = EDGE_LOOP ( 'NONE', ( #4753, #6210, #9112, #2953 ) ) ;
#7643 = ORIENTED_EDGE ( 'NONE', *, *, #463, .T. ) ;
#7644 = CIRCLE ( 'NONE', #15876, 10.00000000000000178 ) ;
#7645 = CARTESIAN_POINT ( 'NONE',  ( 46.99999999999988631, 493.2350855268086320, -508.1801094700848580 ) ) ;
#7646 = ORIENTED_EDGE ( 'NONE', *, *, #13780, .F. ) ;
#7647 = ORIENTED_EDGE ( 'NONE', *, *, #7775, .T. ) ;
#7648 = VERTEX_POINT ( 'NONE', #1600 ) ;
#7649 = LINE ( 'NONE', #2681, #10465 ) ;
#7650 = DIRECTION ( 'NONE',  ( -1.000000000000000000, -0.000000000000000000, -0.000000000000000000 ) ) ;
#7651 = VECTOR ( 'NONE', #2044, 1000.000000000000114 ) ;
#7652 = ORIENTED_EDGE ( 'NONE', *, *, #13536, .F. ) ;
#7653 = DIRECTION ( 'NONE',  ( 1.000000000000000000, 0.000000000000000000, 0.000000000000000000 ) ) ;
#7654 = DIRECTION ( 'NONE',  ( 0.000000000000000000, 0.000000000000000000, -1.000000000000000000 ) ) ;
#7655 = LINE ( 'NONE', #15405, #13140 ) ;
#7656 = CARTESIAN_POINT ( 'NONE',  ( 394.0000000000001137, 240.0523724647196389, -17.15546574335979813 ) ) ;
#7657 = EDGE_LOOP ( 'NONE', ( #6248, #10704, #8280, #8364 ) ) ;
#7658 = LINE ( 'NONE', #9141, #8709 ) ;
#7659 = CARTESIAN_POINT ( 'NONE',  ( -10.00000000000000000, 0.000000000000000000, 0.000000000000000000 ) ) ;
#7660 = ORIENTED_EDGE ( 'NONE', *, *, #6559, .T. ) ;
#7661 = CARTESIAN_POINT ( 'NONE',  ( 25.99999999999996092, 0.000000000000000000, -33.99999999999998579 ) ) ;
#7662 = ORIENTED_EDGE ( 'NONE', *, *, #2311, .F. ) ;
#7663 = LINE ( 'NONE', #6629, #6727 ) ;
#7664 =( GEOMETRIC_REPRESENTATION_CONTEXT ( 3 ) GLOBAL_UNCERTAINTY_ASSIGNED_CONTEXT ( ( #4682 ) ) GLOBAL_UNIT_ASSIGNED_CONTEXT ( ( #11912, #9334, #8034 ) ) REPRESENTATION_CONTEXT ( 'NONE', 'WORKASPACE' ) );
#7665 = VECTOR ( 'NONE', #7619, 1000.000000000000000 ) ;
#7666 = ORIENTED_EDGE ( 'NONE', *, *, #9203, .F. ) ;
#7667 = ORIENTED_EDGE ( 'NONE', *, *, #4661, .T. ) ;
#7668 = FACE_OUTER_BOUND ( 'NONE', #13947, .T. ) ;
#7669 = DIRECTION ( 'NONE',  ( 0.000000000000000000, 0.000000000000000000, 1.000000000000000000 ) ) ;
#7670 = DIRECTION ( 'NONE',  ( -2.920976200236518919E-15, 0.9950371902099891530, 0.09950371902099770793 ) ) ;
#7671 = ORIENTED_EDGE ( 'NONE', *, *, #6231, .F. ) ;
#7672 = EDGE_CURVE ( 'NONE', #9768, #5130, #9507, .T. ) ;
#7673 = CARTESIAN_POINT ( 'NONE',  ( 0.000000000000000000, 0.000000000000000000, 0.000000000000000000 ) ) ;
#7674 = AXIS2_PLACEMENT_3D ( 'NONE', #14098, #14263, #13145 ) ;
#7675 = CARTESIAN_POINT ( 'NONE',  ( -440.0000000000000568, 425.7506394335853201, -11.00000000000000000 ) ) ;
#7676 = SHAPE_REPRESENTATION ( 'Part9^Assem2', ( #1488 ), #14944 ) ;
#7677 = CARTESIAN_POINT ( 'NONE',  ( 17.00000000000000711, 0.000000000000000000, -17.00000000000000355 ) ) ;
#7678 = DIRECTION ( 'NONE',  ( 0.000000000000000000, 0.000000000000000000, 1.000000000000000000 ) ) ;
#7679 = EDGE_CURVE ( 'NONE', #997, #9809, #14748, .T. ) ;
#7680 = PRESENTATION_LAYER_ASSIGNMENT (  '', '', ( #5497 ) ) ;
#7681 = DIRECTION ( 'NONE',  ( 0.000000000000000000, -0.9950371902099891530, -0.09950371902099770793 ) ) ;
#7682 = DIRECTION ( 'NONE',  ( 0.000000000000000000, 1.000000000000000000, 0.000000000000000000 ) ) ;
#7684 = ORIENTED_EDGE ( 'NONE', *, *, #14985, .T. ) ;
#7683 = EDGE_LOOP ( 'NONE', ( #8209, #2632, #13381, #15537 ) ) ;
#7685 = CIRCLE ( 'NONE', #12138, 9.000000000000007105 ) ;
#7686 = DIRECTION ( 'NONE',  ( 1.000000000000000000, 0.000000000000000000, 0.000000000000000000 ) ) ;
#7687 = CIRCLE ( 'NONE', #14840, 60.00000000000002842 ) ;
#7688 = CARTESIAN_POINT ( 'NONE',  ( -46.99999999999988631, 559.9933750504617365, -546.7230258972048205 ) ) ;
#7689 = FACE_OUTER_BOUND ( 'NONE', #9336, .T. ) ;
#7690 = VERTEX_POINT ( 'NONE', #3059 ) ;
#7691 = EDGE_CURVE ( 'NONE', #8443, #8929, #1681, .T. ) ;
#7692 = PLANE ( 'NONE',  #8586 ) ;
#7693 = DIRECTION ( 'NONE',  ( 0.000000000000000000, 0.3746065934159141242, -0.9271838545667866471 ) ) ;
#7694 = EDGE_LOOP ( 'NONE', ( #16145, #4602, #12925, #79 ) ) ;
#7695 = CARTESIAN_POINT ( 'NONE',  ( -22.00000000000001776, 10.00000000000000000, 36.00000000000000711 ) ) ;
#7696 = ADVANCED_FACE ( 'NONE', ( #6740 ), #8126, .T. ) ;
#7697 = CARTESIAN_POINT ( 'NONE',  ( 31.00000000000004263, 68.00000000000000000, -25.99999999999999645 ) ) ;
#7698 = FACE_OUTER_BOUND ( 'NONE', #4149, .T. ) ;
#7699 = EDGE_LOOP ( 'NONE', ( #35, #6808, #14273, #6356 ) ) ;
#7700 = EDGE_CURVE ( 'NONE', #5421, #15647, #6819, .T. ) ;
#7701 = AXIS2_PLACEMENT_3D ( 'NONE', #4164, #9403, #14651 ) ;
#7702 = EDGE_CURVE ( 'NONE', #13088, #414, #317, .T. ) ;
#7703 = ADVANCED_FACE ( 'NONE', ( #57 ), #5540, .F. ) ;
#7704 = LINE ( 'NONE', #13054, #12436 ) ;
#7705 = ORIENTED_EDGE ( 'NONE', *, *, #9630, .T. ) ;
#7706 = ADVANCED_BREP_SHAPE_REPRESENTATION ( '', ( #3164, #1488 ), #16580 ) ;
#7707 = CARTESIAN_POINT ( 'NONE',  ( 31.81980515339464333, 8.000000000000000000, -31.81980515339463622 ) ) ;
#7708 = VECTOR ( 'NONE', #591, 1000.000000000000000 ) ;
#7709 = VECTOR ( 'NONE', #15531, 1000.000000000000000 ) ;
#7710 = CARTESIAN_POINT ( 'NONE',  ( 35.00000000000000711, 8.000000000000000000, -35.00000000000000711 ) ) ;
#7711 = AXIS2_PLACEMENT_3D ( 'NONE', #12631, #4638, #3536 ) ;
#7712 = ORIENTED_EDGE ( 'NONE', *, *, #7306, .T. ) ;
#7713 = DIRECTION ( 'NONE',  ( 1.000000000000000000, -0.000000000000000000, -0.000000000000000000 ) ) ;
#7714 = DIRECTION ( 'NONE',  ( 6.123031769111888756E-17, -1.000000000000000000, -3.749151804555344967E-33 ) ) ;
#7715 = AXIS2_PLACEMENT_3D ( 'NONE', #2732, #11934, #15789 ) ;
#7716 = DIRECTION ( 'NONE',  ( -0.000000000000000000, -1.000000000000000000, -0.000000000000000000 ) ) ;
#7717 = VERTEX_POINT ( 'NONE', #10787 ) ;
#7718 = CARTESIAN_POINT ( 'NONE',  ( -31.00000000000000000, 11.00000000000000000, 30.99999999999999289 ) ) ;
#7719 = CIRCLE ( 'NONE', #622, 2.500000000000002220 ) ;
#7720 = AXIS2_PLACEMENT_3D ( 'NONE', #1370, #13228, #4038 ) ;
#7721 = EDGE_CURVE ( 'NONE', #12617, #12991, #15849, .T. ) ;
#7722 = DIRECTION ( 'NONE',  ( 0.000000000000000000, 0.000000000000000000, -1.000000000000000000 ) ) ;
#7723 = ORIENTED_EDGE ( 'NONE', *, *, #9875, .F. ) ;
#7724 = EDGE_CURVE ( 'NONE', #295, #4908, #10528, .T. ) ;
#7725 = EDGE_CURVE ( 'NONE', #3951, #11607, #15551, .T. ) ;
#7726 = LINE ( 'NONE', #5150, #14647 ) ;
#7727 = ORIENTED_EDGE ( 'NONE', *, *, #7255, .F. ) ;
#7728 = ORIENTED_EDGE ( 'NONE', *, *, #6763, .F. ) ;
#7729 = VECTOR ( 'NONE', #15200, 1000.000000000000000 ) ;
#7730 = DIRECTION ( 'NONE',  ( -1.000000000000000000, 0.000000000000000000, 0.000000000000000000 ) ) ;
#7731 = ORIENTED_EDGE ( 'NONE', *, *, #1086, .T. ) ;
#7732 =( LENGTH_UNIT ( ) NAMED_UNIT ( * ) SI_UNIT ( .MILLI., .METRE. ) );
#7733 = ORIENTED_EDGE ( 'NONE', *, *, #3119, .F. ) ;
#7734 = EDGE_LOOP ( 'NONE', ( #2619, #9810, #13672, #3499 ) ) ;
#7735 = FACE_OUTER_BOUND ( 'NONE', #8862, .T. ) ;
#7736 = CARTESIAN_POINT ( 'NONE',  ( 4.469960816887838430E-15, 3.000000000000000000, 36.50000000000000000 ) ) ;
#7737 = AXIS2_PLACEMENT_3D ( 'NONE', #13309, #14582, #8049 ) ;
#7738 = ORIENTED_EDGE ( 'NONE', *, *, #3185, .F. ) ;
#7739 = DIRECTION ( 'NONE',  ( 0.000000000000000000, 0.000000000000000000, -1.000000000000000000 ) ) ;
#7740 =( LENGTH_UNIT ( ) NAMED_UNIT ( * ) SI_UNIT ( .MILLI., .METRE. ) );
#7741 = VECTOR ( 'NONE', #216, 1000.000000000000000 ) ;
#7742 = DIRECTION ( 'NONE',  ( 0.000000000000000000, 1.000000000000000000, 0.000000000000000000 ) ) ;
#7743 = AXIS2_PLACEMENT_3D ( 'NONE', #13386, #159, #1611 ) ;
#7744 = VERTEX_POINT ( 'NONE', #4091 ) ;
#7745 = CARTESIAN_POINT ( 'NONE',  ( -20.00000000000003197, 0.000000000000000000, 37.00000000000000711 ) ) ;
#7746 = DIRECTION ( 'NONE',  ( 1.196361017915039732E-16, 0.000000000000000000, 1.000000000000000000 ) ) ;
#7747 = ORIENTED_EDGE ( 'NONE', *, *, #6811, .T. ) ;
#7748 = CYLINDRICAL_SURFACE ( 'NONE', #9056, 60.00000000000002842 ) ;
#7749 = ORIENTED_EDGE ( 'NONE', *, *, #12600, .F. ) ;
#7750 = VECTOR ( 'NONE', #4917, 1000.000000000000000 ) ;
#7751 = DIRECTION ( 'NONE',  ( 0.000000000000000000, -1.000000000000000000, 8.952264470854156086E-17 ) ) ;
#7752 = ORIENTED_EDGE ( 'NONE', *, *, #4848, .T. ) ;
#7753 = AXIS2_PLACEMENT_3D ( 'NONE', #2609, #3894, #11789 ) ;
#7754 = EDGE_CURVE ( 'NONE', #2083, #10758, #9798, .T. ) ;
#7755 = ORIENTED_EDGE ( 'NONE', *, *, #11609, .T. ) ;
#7756 = FACE_BOUND ( 'NONE', #16245, .T. ) ;
#7757 = AXIS2_PLACEMENT_3D ( 'NONE', #13698, #3150, #4657 ) ;
#7758 = EDGE_CURVE ( 'NONE', #15921, #2563, #12167, .T. ) ;
#7759 = CARTESIAN_POINT ( 'NONE',  ( -22.00000000000001776, 8.000000000000000000, 36.00000000000000711 ) ) ;
#7760 = DIRECTION ( 'NONE',  ( 0.000000000000000000, 0.000000000000000000, 1.000000000000000000 ) ) ;
#7761 = ORIENTED_EDGE ( 'NONE', *, *, #5841, .F. ) ;
#7762 = CARTESIAN_POINT ( 'NONE',  ( -31.00000000000003197, 3.000000000000000000, -30.99999999999999289 ) ) ;
#7763 = CARTESIAN_POINT ( 'NONE',  ( -46.99999999999988631, 559.9933750504617365, -533.0276205133087615 ) ) ;
#7764 = AXIS2_PLACEMENT_3D ( 'NONE', #7978, #15882, #12034 ) ;
#7765 = CARTESIAN_POINT ( 'NONE',  ( -46.99999999999988631, 549.5810598491749488, -589.0260321808809749 ) ) ;
#7766 = CARTESIAN_POINT ( 'NONE',  ( -26.00000000000002842, 0.000000000000000000, -31.00000000000003197 ) ) ;
#7767 = DIRECTION ( 'NONE',  ( -1.000000000000000000, 0.000000000000000000, -8.673617379884027583E-16 ) ) ;
#7768 = CIRCLE ( 'NONE', #8615, 10.00000000000000178 ) ;
#7769 = CARTESIAN_POINT ( 'NONE',  ( -45.00000000000000000, 515.4878487013597805, -546.7230258972048205 ) ) ;
#7770 = CIRCLE ( 'NONE', #676, 0.7366000000000004766 ) ;
#7771 = DIRECTION ( 'NONE',  ( -1.000000000000000000, -0.000000000000000000, -0.000000000000000000 ) ) ;
#7773 = ORIENTED_EDGE ( 'NONE', *, *, #12048, .F. ) ;
#7772 = ORIENTED_EDGE ( 'NONE', *, *, #12489, .T. ) ;
#7774 = LINE ( 'NONE', #5122, #15228 ) ;
#7775 = EDGE_CURVE ( 'NONE', #7250, #13244, #4011, .T. ) ;
#7776 = VECTOR ( 'NONE', #5886, 1000.000000000000000 ) ;
#7777 = AXIS2_PLACEMENT_3D ( 'NONE', #14952, #608, #16400 ) ;
#7778 = CARTESIAN_POINT ( 'NONE',  ( 31.00000000000003553, 19.00000000000000000, 25.99999999999999645 ) ) ;
#7779 = LINE ( 'NONE', #13040, #6309 ) ;
#7780 = DIRECTION ( 'NONE',  ( 0.000000000000000000, 0.000000000000000000, 1.000000000000000000 ) ) ;
#7781 = EDGE_CURVE ( 'NONE', #2164, #8649, #2181, .T. ) ;
#7782 = ORIENTED_EDGE ( 'NONE', *, *, #6556, .F. ) ;
#7783 = CIRCLE ( 'NONE', #11879, 4.006599999998782913 ) ;
#7784 = CARTESIAN_POINT ( 'NONE',  ( 37.00000000000003553, 3.000000000000000000, 23.00000000000000355 ) ) ;
#7785 = DIRECTION ( 'NONE',  ( 1.000000000000000000, 0.000000000000000000, -0.000000000000000000 ) ) ;
#7786 = ORIENTED_EDGE ( 'NONE', *, *, #7721, .F. ) ;
#7787 = CARTESIAN_POINT ( 'NONE',  ( 0.000000000000000000, -156.2292101480469739, -357.0417483806770633 ) ) ;
#7788 = FACE_OUTER_BOUND ( 'NONE', #7820, .T. ) ;
#7789 = CARTESIAN_POINT ( 'NONE',  ( 0.000000000000000000, 341.0487089519837696, -96.50000000000331113 ) ) ;
#7790 = ORIENTED_EDGE ( 'NONE', *, *, #12710, .F. ) ;
#7791 = SURFACE_STYLE_FILL_AREA ( #2564 ) ;
#7792 = FACE_OUTER_BOUND ( 'NONE', #3528, .T. ) ;
#7793 = CARTESIAN_POINT ( 'NONE',  ( -34.99999999999996447, 8.000000000000000000, -40.00000000000000711 ) ) ;
#7794 = ORIENTED_EDGE ( 'NONE', *, *, #7000, .F. ) ;
#7795 = CARTESIAN_POINT ( 'NONE',  ( 46.99999999999988631, 549.5810598491749488, -575.3306267969850296 ) ) ;
#7796 = ORIENTED_EDGE ( 'NONE', *, *, #6138, .T. ) ;
#7797 = EDGE_CURVE ( 'NONE', #5489, #16470, #1287, .T. ) ;
#7798 = ADVANCED_FACE ( 'NONE', ( #5883 ), #3482, .F. ) ;
#7799 = CONTEXT_DEPENDENT_SHAPE_REPRESENTATION ( #207, #16186 ) ;
#7800 =( NAMED_UNIT ( * ) PLANE_ANGLE_UNIT ( ) SI_UNIT ( $, .RADIAN. ) );
#7801 = VECTOR ( 'NONE', #12803, 1000.000000000000000 ) ;
#7802 = EDGE_CURVE ( 'NONE', #10409, #15631, #16905, .T. ) ;
#7803 = DIRECTION ( 'NONE',  ( 0.000000000000000000, 0.000000000000000000, -1.000000000000000000 ) ) ;
#7804 = EDGE_CURVE ( 'NONE', #3015, #15220, #16365, .T. ) ;
#7805 = ORIENTED_EDGE ( 'NONE', *, *, #5727, .F. ) ;
#7806 = EDGE_CURVE ( 'NONE', #6882, #1506, #13633, .T. ) ;
#7807 = FACE_BOUND ( 'NONE', #4621, .T. ) ;
#7808 = CARTESIAN_POINT ( 'NONE',  ( 56.73000000000000398, 261.2094592450224582, 287.2045212030221251 ) ) ;
#7809 = DIRECTION ( 'NONE',  ( 0.000000000000000000, 0.000000000000000000, -1.000000000000000000 ) ) ;
#7810 = VERTEX_POINT ( 'NONE', #743 ) ;
#7811 = FACE_OUTER_BOUND ( 'NONE', #15753, .T. ) ;
#7812 = DIRECTION ( 'NONE',  ( -0.000000000000000000, 1.000000000000000000, -0.000000000000000000 ) ) ;
#7813 = VERTEX_POINT ( 'NONE', #15073 ) ;
#7814 = AXIS2_PLACEMENT_3D ( 'NONE', #1432, #13205, #14495 ) ;
#7815 = DIRECTION ( 'NONE',  ( -0.000000000000000000, 1.000000000000000000, -0.000000000000000000 ) ) ;
#7816 = ORIENTED_EDGE ( 'NONE', *, *, #9415, .T. ) ;
#7817 = ORIENTED_EDGE ( 'NONE', *, *, #13293, .T. ) ;
#7818 = CARTESIAN_POINT ( 'NONE',  ( -20.00000000000003197, 0.000000000000000000, 37.00000000000000711 ) ) ;
#7819 = EDGE_CURVE ( 'NONE', #2588, #16404, #12276, .T. ) ;
#7820 = EDGE_LOOP ( 'NONE', ( #4496, #15723, #1345, #14814 ) ) ;
#7821 = CARTESIAN_POINT ( 'NONE',  ( 439.9999999999998295, -240.7506394335853201, -185.0000000000000000 ) ) ;
#7822 = ORIENTED_EDGE ( 'NONE', *, *, #16414, .F. ) ;
#7823 = EDGE_CURVE ( 'NONE', #11352, #2454, #3310, .T. ) ;
#7824 = EDGE_CURVE ( 'NONE', #2782, #6058, #7574, .T. ) ;
#7825 = VECTOR ( 'NONE', #11017, 1000.000000000000227 ) ;
#7826 = EDGE_CURVE ( 'NONE', #5640, #10374, #491, .T. ) ;
#7827 = VERTEX_POINT ( 'NONE', #12257 ) ;
#7828 = AXIS2_PLACEMENT_3D ( 'NONE', #15838, #9238, #4079 ) ;
#7829 = EDGE_CURVE ( 'NONE', #3064, #16287, #3218, .T. ) ;
#7830 = CARTESIAN_POINT ( 'NONE',  ( 31.00000000000000000, 8.000000000000000000, 30.99999999999999289 ) ) ;
#7831 = DIRECTION ( 'NONE',  ( 0.000000000000000000, 0.000000000000000000, -1.000000000000000000 ) ) ;
#7832 = ORIENTED_EDGE ( 'NONE', *, *, #263, .F. ) ;
#7833 = DIRECTION ( 'NONE',  ( -0.000000000000000000, -1.000000000000000000, -0.000000000000000000 ) ) ;
#7834 = DIRECTION ( 'NONE',  ( 0.000000000000000000, 0.09950371902099953980, 0.9950371902099890420 ) ) ;
#7835 = CARTESIAN_POINT ( 'NONE',  ( -440.0000000000000568, 620.7506394335853201, -11.00000000000000000 ) ) ;
#7836 = ORIENTED_EDGE ( 'NONE', *, *, #2335, .T. ) ;
#7837 = CARTESIAN_POINT ( 'NONE',  ( -430.0000000000000568, 620.7506394335853201, 109.9999999999999858 ) ) ;
#7838 = CARTESIAN_POINT ( 'NONE',  ( 17.00000000000000711, 277.8092731128509740, -29.71049682360898103 ) ) ;
#7839 = ORIENTED_EDGE ( 'NONE', *, *, #1223, .T. ) ;
#7840 = AXIS2_PLACEMENT_3D ( 'NONE', #191, #12117, #4473 ) ;
#7841 = VECTOR ( 'NONE', #6403, 1000.000000000000000 ) ;
#7842 = DIRECTION ( 'NONE',  ( -1.000000000000000000, -0.000000000000000000, -0.000000000000000000 ) ) ;
#7843 = EDGE_LOOP ( 'NONE', ( #13592, #10774, #13364, #6624 ) ) ;
#7844 = DIRECTION ( 'NONE',  ( 0.000000000000000000, -0.000000000000000000, 1.000000000000000000 ) ) ;
#7845 = VERTEX_POINT ( 'NONE', #12412 ) ;
#7846 = ORIENTED_EDGE ( 'NONE', *, *, #5298, .F. ) ;
#7847 = CARTESIAN_POINT ( 'NONE',  ( 46.99999999999988631, 559.9933750504617365, -551.4184312811007658 ) ) ;
#7848 = LINE ( 'NONE', #15420, #6378 ) ;
#7849 = VECTOR ( 'NONE', #6645, 1000.000000000000000 ) ;
#7850 = EDGE_LOOP ( 'NONE', ( #1742, #5170 ) ) ;
#7851 = AXIS2_PLACEMENT_3D ( 'NONE', #9859, #10972, #12594 ) ;
#7852 = DIRECTION ( 'NONE',  ( 0.000000000000000000, 1.000000000000000000, 0.000000000000000000 ) ) ;
#7853 = DIRECTION ( 'NONE',  ( 1.000000000000000000, 0.000000000000000000, -0.000000000000000000 ) ) ;
#7854 = DIRECTION ( 'NONE',  ( 0.000000000000000000, 0.000000000000000000, 1.000000000000000000 ) ) ;
#7855 =( REPRESENTATION_RELATIONSHIP ('NONE','NONE', #15822, #6937 ) REPRESENTATION_RELATIONSHIP_WITH_TRANSFORMATION ( #5893 )SHAPE_REPRESENTATION_RELATIONSHIP( ) );
#7856 = FACE_BOUND ( 'NONE', #10940, .T. ) ;
#7857 = DIRECTION ( 'NONE',  ( 0.000000000000000000, 0.000000000000000000, -1.000000000000000000 ) ) ;
#7858 = DIRECTION ( 'NONE',  ( 0.000000000000000000, 0.000000000000000000, -1.000000000000000000 ) ) ;
#7859 = CARTESIAN_POINT ( 'NONE',  ( 30.99999999999999645, 0.000000000000000000, 26.00000000000000355 ) ) ;
#7860 = EDGE_CURVE ( 'NONE', #7626, #13903, #10902, .T. ) ;
#7862 = ORIENTED_EDGE ( 'NONE', *, *, #13902, .T. ) ;
#7861 = ORIENTED_EDGE ( 'NONE', *, *, #12053, .F. ) ;
#7863 = AXIS2_PLACEMENT_3D ( 'NONE', #11456, #10173, #10854 ) ;
#7864 = CARTESIAN_POINT ( 'NONE',  ( 35.00000000000003553, 3.000000000000000000, -23.50000000000000000 ) ) ;
#7865 = CIRCLE ( 'NONE', #5950, 3.000000000000002665 ) ;
#7866 = EDGE_CURVE ( 'NONE', #11485, #10332, #2012, .T. ) ;
#7867 = DIRECTION ( 'NONE',  ( 0.000000000000000000, 0.000000000000000000, -1.000000000000000000 ) ) ;
#7868 = LINE ( 'NONE', #1436, #7967 ) ;
#7869 = LINE ( 'NONE', #11826, #15437 ) ;
#7870 = EDGE_LOOP ( 'NONE', ( #11558, #8074, #13179, #10675 ) ) ;
#7871 = DIRECTION ( 'NONE',  ( -1.000000000000000000, 0.000000000000000000, 0.000000000000000000 ) ) ;
#7872 = MECHANICAL_DESIGN_GEOMETRIC_PRESENTATION_REPRESENTATION (  '', ( #7055 ), #212 ) ;
#7873 = PRODUCT_RELATED_PRODUCT_CATEGORY ( 'part', '', ( #1810 ) ) ;
#7874 = DIRECTION ( 'NONE',  ( 0.000000000000000000, -1.000000000000000000, 2.220446049250308742E-15 ) ) ;
#7875 = ORIENTED_EDGE ( 'NONE', *, *, #15354, .F. ) ;
#7876 = CARTESIAN_POINT ( 'NONE',  ( 1.347066989204613998E-15, 0.000000000000000000, 22.00000000000000000 ) ) ;
#7877 = FACE_OUTER_BOUND ( 'NONE', #1466, .T. ) ;
#7878 = CARTESIAN_POINT ( 'NONE',  ( -31.00000000000003197, 3.000000000000000000, -30.99999999999999289 ) ) ;
#7879 = CARTESIAN_POINT ( 'NONE',  ( 17.00000000000000000, 380.0000000000000000, -75.00000000000000000 ) ) ;
#7880 = FACE_OUTER_BOUND ( 'NONE', #8187, .T. ) ;
#7881 = CARTESIAN_POINT ( 'NONE',  ( 35.00000000000003553, 3.000000000000000000, -18.49999999999999645 ) ) ;
#7882 = ORIENTED_EDGE ( 'NONE', *, *, #1000, .F. ) ;
#7883 = ADVANCED_FACE ( 'NONE', ( #7244 ), #651, .T. ) ;
#7884 = DIRECTION ( 'NONE',  ( -1.000000000000000000, 0.000000000000000000, 0.000000000000000000 ) ) ;
#7885 = CONTEXT_DEPENDENT_SHAPE_REPRESENTATION ( #1394, #13731 ) ;
#7886 = AXIS2_PLACEMENT_3D ( 'NONE', #1540, #1800, #12278 ) ;
#7887 =( NAMED_UNIT ( * ) SI_UNIT ( $, .STERADIAN. ) SOLID_ANGLE_UNIT ( ) );
#7888 = DIRECTION ( 'NONE',  ( -0.000000000000000000, -1.000000000000000000, -0.000000000000000000 ) ) ;
#7889 = VERTEX_POINT ( 'NONE', #9921 ) ;
#7890 = PLANE ( 'NONE',  #346 ) ;
#7891 = DIRECTION ( 'NONE',  ( -0.000000000000000000, 1.000000000000000000, -0.000000000000000000 ) ) ;
#7892 = EDGE_CURVE ( 'NONE', #13622, #11999, #5796, .T. ) ;
#7893 = CARTESIAN_POINT ( 'NONE',  ( 65.00000000000000000, 0.000000000000000000, -7.000000000000006217 ) ) ;
#7894 = ORIENTED_EDGE ( 'NONE', *, *, #8262, .T. ) ;
#7895 = DIRECTION ( 'NONE',  ( 1.000000000000000000, 0.000000000000000000, 0.000000000000000000 ) ) ;
#7896 = CARTESIAN_POINT ( 'NONE',  ( -3.270000000000002238, 239.4632308570078294, 56.73739990498292940 ) ) ;
#7897 = DIRECTION ( 'NONE',  ( 0.000000000000000000, 0.000000000000000000, 1.000000000000000000 ) ) ;
#7898 = ORIENTED_EDGE ( 'NONE', *, *, #65, .F. ) ;
#7899 = FACE_OUTER_BOUND ( 'NONE', #10475, .T. ) ;
#7900 = ORIENTED_EDGE ( 'NONE', *, *, #8266, .F. ) ;
#7901 = ORIENTED_EDGE ( 'NONE', *, *, #7724, .F. ) ;
#7902 = EDGE_CURVE ( 'NONE', #9126, #4738, #11041, .T. ) ;
#7903 = FACE_OUTER_BOUND ( 'NONE', #7117, .T. ) ;
#7904 = ORIENTED_EDGE ( 'NONE', *, *, #2675, .F. ) ;
#7905 = ORIENTED_EDGE ( 'NONE', *, *, #15287, .F. ) ;
#7906 = DIRECTION ( 'NONE',  ( 1.000000000000000000, 0.000000000000000000, 0.000000000000000000 ) ) ;
#7907 = ORIENTED_EDGE ( 'NONE', *, *, #5095, .F. ) ;
#7908 = EDGE_LOOP ( 'NONE', ( #2584, #15579, #3396, #3934 ) ) ;
#7909 = DIRECTION ( 'NONE',  ( 7.900838015626929923E-17, 8.586860021784410058E-33, -1.000000000000000000 ) ) ;
#7910 = DIRECTION ( 'NONE',  ( 1.000000000000000000, -0.000000000000000000, -0.000000000000000000 ) ) ;
#7911 = ADVANCED_FACE ( 'NONE', ( #8641 ), #2101, .T. ) ;
#7912 = ORIENTED_EDGE ( 'NONE', *, *, #5874, .T. ) ;
#7913 = DIRECTION ( 'NONE',  ( 0.000000000000000000, 0.9161352426163912321, -0.4008693268837190127 ) ) ;
#7914 = CARTESIAN_POINT ( 'NONE',  ( 5.687501635565830327, 0.000000000000000000, 0.000000000000000000 ) ) ;
#7915 = ORIENTED_EDGE ( 'NONE', *, *, #13616, .F. ) ;
#7916 = CIRCLE ( 'NONE', #4098, 25.00000000000002132 ) ;
#7917 = DIRECTION ( 'NONE',  ( -1.000000000000000000, -0.000000000000000000, -0.000000000000000000 ) ) ;
#7918 = EDGE_CURVE ( 'NONE', #3171, #13742, #7152, .T. ) ;
#7919 = ORIENTED_EDGE ( 'NONE', *, *, #11829, .F. ) ;
#7920 = CARTESIAN_POINT ( 'NONE',  ( -54.99999999999999289, 515.4878487013597805, -734.2230258972047068 ) ) ;
#7921 = CARTESIAN_POINT ( 'NONE',  ( -31.00000000000006750, 3.000000000000000000, 26.00000000000000355 ) ) ;
#7922 = EDGE_LOOP ( 'NONE', ( #8142, #2048, #14367, #14424, #3046 ) ) ;
#7923 = ADVANCED_FACE ( 'NONE', ( #2348 ), #7315, .T. ) ;
#7924 = EDGE_CURVE ( 'NONE', #10121, #10620, #8891, .T. ) ;
#7925 = EDGE_CURVE ( 'NONE', #1685, #13387, #12662, .T. ) ;
#7926 = CARTESIAN_POINT ( 'NONE',  ( -46.99999999999988631, 523.2161522479893847, -595.2478186815853860 ) ) ;
#7927 = VERTEX_POINT ( 'NONE', #5092 ) ;
#7928 = LINE ( 'NONE', #9398, #13620 ) ;
#7929 = EDGE_LOOP ( 'NONE', ( #12201, #3470, #4818, #9557 ) ) ;
#7930 = VECTOR ( 'NONE', #14945, 1000.000000000000000 ) ;
#7931 = VERTEX_POINT ( 'NONE', #16860 ) ;
#7932 = DIRECTION ( 'NONE',  ( -0.000000000000000000, 0.4008693268837190127, 0.9161352426163912321 ) ) ;
#7933 = CARTESIAN_POINT ( 'NONE',  ( 56.73000000000001108, 286.2094592450221739, 37.20452120302225296 ) ) ;
#7934 = DIRECTION ( 'NONE',  ( -1.000000000000000000, -0.000000000000000000, 3.854941057726258312E-16 ) ) ;
#7935 = ORIENTED_EDGE ( 'NONE', *, *, #13839, .F. ) ;
#7936 = CARTESIAN_POINT ( 'NONE',  ( 25.99999999999998224, 6.000000000000000000, -31.99999999999998579 ) ) ;
#7937 = PRODUCT_DEFINITION_SHAPE ( 'NONE', 'NONE',  #16973 ) ;
#7938 = FACE_OUTER_BOUND ( 'NONE', #5844, .T. ) ;
#7939 = PLANE ( 'NONE',  #4411 ) ;
#7940 = DIRECTION ( 'NONE',  ( -0.000000000000000000, 1.000000000000000000, 0.000000000000000000 ) ) ;
#7941 = DIRECTION ( 'NONE',  ( -1.000000000000000000, -0.000000000000000000, -0.000000000000000000 ) ) ;
#7942 = CIRCLE ( 'NONE', #16718, 4.695405383896011919 ) ;
#7943 = AXIS2_PLACEMENT_3D ( 'NONE', #16210, #15266, #1873 ) ;
#7944 = EDGE_CURVE ( 'NONE', #15084, #4897, #3488, .T. ) ;
#7945 = CARTESIAN_POINT ( 'NONE',  ( -23.00000000000002132, 6.000000000000000000, 37.00000000000000711 ) ) ;
#7946 = CARTESIAN_POINT ( 'NONE',  ( 21.99999999999998224, 8.000000000000000000, -32.99999999999999289 ) ) ;
#7948 = VERTEX_POINT ( 'NONE', #13007 ) ;
#7947 = VERTEX_POINT ( 'NONE', #7745 ) ;
#7949 = DIRECTION ( 'NONE',  ( -0.000000000000000000, -1.000000000000000000, 0.000000000000000000 ) ) ;
#7950 = PRESENTATION_LAYER_ASSIGNMENT (  '', '', ( #14543 ) ) ;
#7951 = DIRECTION ( 'NONE',  ( -1.000000000000000000, -0.000000000000000000, -1.631319816340925608E-17 ) ) ;
#7952 = DIRECTION ( 'NONE',  ( 0.000000000000000000, 0.000000000000000000, -1.000000000000000000 ) ) ;
#7953 = DIRECTION ( 'NONE',  ( -0.000000000000000000, 1.000000000000000000, -0.000000000000000000 ) ) ;
#7954 = CIRCLE ( 'NONE', #571, 22.50000000000000000 ) ;
#7955 = ORIENTED_EDGE ( 'NONE', *, *, #15990, .F. ) ;
#7956 = AXIS2_PLACEMENT_3D ( 'NONE', #10527, #10616, #54 ) ;
#7957 = DIRECTION ( 'NONE',  ( 0.000000000000000000, 0.000000000000000000, -1.000000000000000000 ) ) ;
#7958 = APPLICATION_CONTEXT ( 'automotive_design' ) ;
#7959 = CARTESIAN_POINT ( 'NONE',  ( 44.68009836720081296, 275.4439001176564830, 0.000000000000000000 ) ) ;
#7960 = VERTEX_POINT ( 'NONE', #6124 ) ;
#7961 = FACE_OUTER_BOUND ( 'NONE', #11711, .T. ) ;
#7962 = CARTESIAN_POINT ( 'NONE',  ( -54.99999999999999289, 515.4878487013597805, -546.7230258972048205 ) ) ;
#7963 = VERTEX_POINT ( 'NONE', #8974 ) ;
#7964 = DIRECTION ( 'NONE',  ( -1.000000000000000000, -0.000000000000000000, -0.000000000000000000 ) ) ;
#7965 = DIRECTION ( 'NONE',  ( 0.000000000000000000, 0.000000000000000000, -1.000000000000000000 ) ) ;
#7966 = ORIENTED_EDGE ( 'NONE', *, *, #350, .T. ) ;
#7967 = VECTOR ( 'NONE', #243, 1000.000000000000000 ) ;
#7968 = CARTESIAN_POINT ( 'NONE',  ( 25.99999999999998224, 8.000000000000000000, -32.99999999999999289 ) ) ;
#7969 = FACE_OUTER_BOUND ( 'NONE', #3778, .T. ) ;
#7970 = MECHANICAL_DESIGN_GEOMETRIC_PRESENTATION_REPRESENTATION (  '', ( #5497 ), #15944 ) ;
#7971 = DIRECTION ( 'NONE',  ( 3.854941057726254860E-16, 0.000000000000000000, -1.000000000000000000 ) ) ;
#7972 = ORIENTED_EDGE ( 'NONE', *, *, #2167, .T. ) ;
#7973 = DIRECTION ( 'NONE',  ( 0.000000000000000000, 0.000000000000000000, 1.000000000000000000 ) ) ;
#7974 = DIRECTION ( 'NONE',  ( -0.000000000000000000, -1.000000000000000000, -0.000000000000000000 ) ) ;
#7975 = TOROIDAL_SURFACE ( 'NONE', #4695, 4.695405383895982609, 9.000000000000000000 ) ;
#7976 = FACE_OUTER_BOUND ( 'NONE', #5590, .T. ) ;
#7977 = ORIENTED_EDGE ( 'NONE', *, *, #14943, .F. ) ;
#7978 = CARTESIAN_POINT ( 'NONE',  ( -1.776356839400249676E-15, 15.90000000000000036, 0.000000000000000000 ) ) ;
#7979 = CARTESIAN_POINT ( 'NONE',  ( -23.00000000000003197, 3.000000000000000000, 37.00000000000000711 ) ) ;
#7980 = CARTESIAN_POINT ( 'NONE',  ( 23.00000000000000711, 68.00000000000000000, -31.00000000000002487 ) ) ;
#7981 = VERTEX_POINT ( 'NONE', #2511 ) ;
#7982 = LINE ( 'NONE', #11955, #2856 ) ;
#7983 = ORIENTED_EDGE ( 'NONE', *, *, #16211, .T. ) ;
#7984 = VERTEX_POINT ( 'NONE', #12910 ) ;
#7985 = DIRECTION ( 'NONE',  ( 1.000000000000000000, 0.000000000000000000, 0.000000000000000000 ) ) ;
#7986 = ORIENTED_EDGE ( 'NONE', *, *, #6139, .F. ) ;
#7987 = SHAPE_DEFINITION_REPRESENTATION ( #7368, #11761 ) ;
#7988 = AXIS2_PLACEMENT_3D ( 'NONE', #8794, #8536, #11274 ) ;
#7989 = EDGE_CURVE ( 'NONE', #11248, #14244, #11989, .T. ) ;
#7990 = ORIENTED_EDGE ( 'NONE', *, *, #14774, .F. ) ;
#7991 = VECTOR ( 'NONE', #10719, 1000.000000000000000 ) ;
#7992 = ORIENTED_EDGE ( 'NONE', *, *, #10017, .F. ) ;
#7993 = AXIS2_PLACEMENT_3D ( 'NONE', #11931, #12096, #6677 ) ;
#7994 = AXIS2_PLACEMENT_3D ( 'NONE', #7688, #12861, #3930 ) ;
#7995 = CARTESIAN_POINT ( 'NONE',  ( 394.0000000000001137, 240.7889724647196488, -17.15546574335979813 ) ) ;
#7996 = DIRECTION ( 'NONE',  ( -0.000000000000000000, -0.000000000000000000, 1.000000000000000000 ) ) ;
#7997 = EDGE_CURVE ( 'NONE', #15120, #16566, #2264, .T. ) ;
#7998 = VERTEX_POINT ( 'NONE', #9050 ) ;
#7999 = CARTESIAN_POINT ( 'NONE',  ( 10.00000000000000000, 435.2933666400819561, -550.3792044179907634 ) ) ;
#8000 = DIRECTION ( 'NONE',  ( 0.000000000000000000, 0.000000000000000000, 1.000000000000000000 ) ) ;
#8001 = ORIENTED_EDGE ( 'NONE', *, *, #12530, .F. ) ;
#8002 = AXIS2_PLACEMENT_3D ( 'NONE', #5142, #3961, #5221 ) ;
#8003 = LINE ( 'NONE', #11882, #6653 ) ;
#8004 = EDGE_LOOP ( 'NONE', ( #15926, #6839, #12795, #9885 ) ) ;
#8005 = CARTESIAN_POINT ( 'NONE',  ( 0.000000000000000000, 309.2289037985885898, -79.88019484660914316 ) ) ;
#8006 = CARTESIAN_POINT ( 'NONE',  ( -55.99999999999989342, 473.6663340069158039, -566.6402177818052905 ) ) ;
#8007 = VERTEX_POINT ( 'NONE', #14210 ) ;
#8008 = CIRCLE ( 'NONE', #12969, 2.500000000000002220 ) ;
#8009 = AXIS2_PLACEMENT_3D ( 'NONE', #10033, #4691, #13977 ) ;
#8010 = CIRCLE ( 'NONE', #4990, 34.00000000000000000 ) ;
#8011 = DIRECTION ( 'NONE',  ( 0.000000000000000000, 0.000000000000000000, 1.000000000000000000 ) ) ;
#8012 = EDGE_LOOP ( 'NONE', ( #2001, #2224, #3128, #13466 ) ) ;
#8013 = DIRECTION ( 'NONE',  ( 1.476083657435421627E-31, -1.000000000000000000, 0.000000000000000000 ) ) ;
#8014 = LINE ( 'NONE', #5616, #14151 ) ;
#8015 = ADVANCED_FACE ( 'NONE', ( #1239, #15652 ), #10264, .F. ) ;
#8016 = ORIENTED_EDGE ( 'NONE', *, *, #12880, .F. ) ;
#8017 = CIRCLE ( 'NONE', #12155, 2.500000000000002220 ) ;
#8018 = VERTEX_POINT ( 'NONE', #6451 ) ;
#8019 = CARTESIAN_POINT ( 'NONE',  ( 0.3499999999999999778, 0.000000000000000000, 0.000000000000000000 ) ) ;
#8020 = EDGE_CURVE ( 'NONE', #9955, #4912, #16938, .T. ) ;
#8021 = LINE ( 'NONE', #397, #13280 ) ;
#8023 = ORIENTED_EDGE ( 'NONE', *, *, #14583, .T. ) ;
#8022 = EDGE_CURVE ( 'NONE', #10332, #7313, #11374, .T. ) ;
#8025 = EDGE_CURVE ( 'NONE', #8101, #7626, #7658, .T. ) ;
#8024 = CARTESIAN_POINT ( 'NONE',  ( 10.00000000000000000, 435.2933666400819561, -575.6295912558023247 ) ) ;
#8026 = AXIS2_PLACEMENT_3D ( 'NONE', #3398, #8642, #13873 ) ;
#8027 = AXIS2_PLACEMENT_3D ( 'NONE', #1270, #5199, #15608 ) ;
#8028 = CARTESIAN_POINT ( 'NONE',  ( 0.000000000000000000, 19.00100000000000122, 0.000000000000000000 ) ) ;
#8029 = LINE ( 'NONE', #13373, #2754 ) ;
#8030 = DIRECTION ( 'NONE',  ( 0.000000000000000000, 0.000000000000000000, -1.000000000000000000 ) ) ;
#8031 = CARTESIAN_POINT ( 'NONE',  ( -26.00000000000000000, 19.00000000000000000, 40.00000000000001421 ) ) ;
#8032 = AXIS2_PLACEMENT_3D ( 'NONE', #9045, #14283, #13001 ) ;
#8033 = CARTESIAN_POINT ( 'NONE',  ( -33.99999999999997158, -20.00000000000000000, -22.99999999999999645 ) ) ;
#8034 =( NAMED_UNIT ( * ) SI_UNIT ( $, .STERADIAN. ) SOLID_ANGLE_UNIT ( ) );
#8036 = VERTEX_POINT ( 'NONE', #2429 ) ;
#8035 = ORIENTED_EDGE ( 'NONE', *, *, #5257, .F. ) ;
#8037 = CIRCLE ( 'NONE', #8314, 7.500000000000000000 ) ;
#8038 = AXIS2_PLACEMENT_3D ( 'NONE', #14225, #7853, #6554 ) ;
#8039 = CIRCLE ( 'NONE', #8872, 14.76997474683060041 ) ;
#8040 = VECTOR ( 'NONE', #3751, 1000.000000000000114 ) ;
#8041 = CARTESIAN_POINT ( 'NONE',  ( 0.6401637624220996026, 286.2061364468225975, 37.23774918501653985 ) ) ;
#8042 = DIRECTION ( 'NONE',  ( 0.000000000000000000, 0.000000000000000000, -1.000000000000000000 ) ) ;
#8043 = EDGE_CURVE ( 'NONE', #7717, #16161, #6200, .T. ) ;
#8044 = FACE_OUTER_BOUND ( 'NONE', #9036, .T. ) ;
#8045 = AXIS2_PLACEMENT_3D ( 'NONE', #10831, #6857, #12115 ) ;
#8046 = EDGE_CURVE ( 'NONE', #3745, #2354, #12834, .T. ) ;
#8047 = ORIENTED_EDGE ( 'NONE', *, *, #714, .T. ) ;
#8048 = EDGE_CURVE ( 'NONE', #15132, #14037, #7579, .T. ) ;
#8049 = DIRECTION ( 'NONE',  ( 0.000000000000000000, 0.000000000000000000, -1.000000000000000000 ) ) ;
#8050 = AXIS2_PLACEMENT_3D ( 'NONE', #3212, #632, #3375 ) ;
#8051 = AXIS2_PLACEMENT_3D ( 'NONE', #6994, #12248, #14907 ) ;
#8052 = DIRECTION ( 'NONE',  ( 0.000000000000000000, -0.6427876096865372535, 0.7660444431189797898 ) ) ;
#8053 = ORIENTED_EDGE ( 'NONE', *, *, #65, .T. ) ;
#8054 = DIRECTION ( 'NONE',  ( 0.000000000000000000, 1.224646799147356165E-16, 1.000000000000000000 ) ) ;
#8055 = VECTOR ( 'NONE', #2602, 1000.000000000000000 ) ;
#8056 = FACE_OUTER_BOUND ( 'NONE', #8911, .T. ) ;
#8057 = DIRECTION ( 'NONE',  ( 5.782411586589399054E-16, 0.000000000000000000, -1.000000000000000000 ) ) ;
#8058 = CIRCLE ( 'NONE', #13831, 0.7366000000000004766 ) ;
#8059 = LINE ( 'NONE', #172, #2544 ) ;
#8060 = SURFACE_SIDE_STYLE ('',( #13654 ) ) ;
#8061 = FACE_OUTER_BOUND ( 'NONE', #16789, .T. ) ;
#8062 = ORIENTED_EDGE ( 'NONE', *, *, #1634, .T. ) ;
#8063 = AXIS2_PLACEMENT_3D ( 'NONE', #7259, #13130, #6242 ) ;
#8064 = EDGE_CURVE ( 'NONE', #365, #8449, #11626, .T. ) ;
#8065 = COLOUR_RGB ( '', 0.72549020, 0.75294118, 0.79215686) ;
#8066 = LINE ( 'NONE', #10990, #815 ) ;
#8067 = FACE_OUTER_BOUND ( 'NONE', #3856, .T. ) ;
#8068 = VERTEX_POINT ( 'NONE', #3739 ) ;
#8069 = VECTOR ( 'NONE', #10490, 1000.000000000000000 ) ;
#8070 = PLANE ( 'NONE',  #11033 ) ;
#8071 = UNCERTAINTY_MEASURE_WITH_UNIT (LENGTH_MEASURE( 1.000000000000000082E-05 ), #8513, 'distance_accuracy_value', 'NONE');
#8072 = CARTESIAN_POINT ( 'NONE',  ( 0.7366000000000293424, 218.4499468633031825, 287.1312267635914850 ) ) ;
#8073 = DIRECTION ( 'NONE',  ( 1.000000000000000000, 0.000000000000000000, -0.000000000000000000 ) ) ;
#8074 = ORIENTED_EDGE ( 'NONE', *, *, #14982, .F. ) ;
#8075 = DIRECTION ( 'NONE',  ( 0.000000000000000000, 0.000000000000000000, 1.000000000000000000 ) ) ;
#8076 = DIRECTION ( 'NONE',  ( -1.000000000000000000, -0.000000000000000000, -0.000000000000000000 ) ) ;
#8077 = FACE_OUTER_BOUND ( 'NONE', #2892, .T. ) ;
#8078 = ORIENTED_EDGE ( 'NONE', *, *, #7355, .F. ) ;
#8079 = FILL_AREA_STYLE_COLOUR ( '', #8344 ) ;
#8080 = VECTOR ( 'NONE', #7891, 1000.000000000000000 ) ;
#8081 = ORIENTED_EDGE ( 'NONE', *, *, #4134, .T. ) ;
#8082 = ORIENTED_EDGE ( 'NONE', *, *, #10790, .T. ) ;
#8083 = EDGE_CURVE ( 'NONE', #3987, #4477, #15282, .T. ) ;
#8084 = CARTESIAN_POINT ( 'NONE',  ( -26.00000000000000000, 11.00000000000000000, -31.00000000000003908 ) ) ;
#8085 = AXIS2_PLACEMENT_3D ( 'NONE', #13735, #516, #7271 ) ;
#8086 = EDGE_LOOP ( 'NONE', ( #9796, #4277 ) ) ;
#8088 = EDGE_CURVE ( 'NONE', #2563, #7469, #384, .T. ) ;
#8087 = AXIS2_PLACEMENT_3D ( 'NONE', #5737, #9702, #8575 ) ;
#8089 = DIRECTION ( 'NONE',  ( 1.000000000000000000, 0.000000000000000000, 0.000000000000000000 ) ) ;
#8090 = PRODUCT_DEFINITION_SHAPE ( 'NONE', 'NONE',  #13469 ) ;
#8091 = ORIENTED_EDGE ( 'NONE', *, *, #2606, .F. ) ;
#8092 = EDGE_CURVE ( 'NONE', #7606, #4921, #4247, .T. ) ;
#8093 = ORIENTED_EDGE ( 'NONE', *, *, #10955, .F. ) ;
#8094 = CARTESIAN_POINT ( 'NONE',  ( -55.99999999999988631, 459.5014304922595443, -192.4166442068759579 ) ) ;
#8095 = CARTESIAN_POINT ( 'NONE',  ( -39.99999999999997868, 3.000000000000000000, 26.00000000000000355 ) ) ;
#8096 =( REPRESENTATION_RELATIONSHIP ('NONE','NONE', #15277, #135 ) REPRESENTATION_RELATIONSHIP_WITH_TRANSFORMATION ( #4895 )SHAPE_REPRESENTATION_RELATIONSHIP( ) );
#8097 = ORIENTED_EDGE ( 'NONE', *, *, #9569, .T. ) ;
#8098 = CIRCLE ( 'NONE', #14414, 4.999999999999997335 ) ;
#8099 = FACE_OUTER_BOUND ( 'NONE', #11727, .T. ) ;
#8100 = DIRECTION ( 'NONE',  ( 1.000000000000000000, 0.000000000000000000, 0.000000000000000000 ) ) ;
#8101 = VERTEX_POINT ( 'NONE', #4337 ) ;
#8102 = PRODUCT_DEFINITION ( 'UNKNOWN', '', #3984, #434 ) ;
#8103 = ORIENTED_EDGE ( 'NONE', *, *, #6438, .T. ) ;
#8104 = DIRECTION ( 'NONE',  ( -1.000000000000000000, 0.000000000000000000, -0.000000000000000000 ) ) ;
#8105 = DIRECTION ( 'NONE',  ( -0.003530072958128175308, -0.9999937692730440641, -1.224639168707530015E-16 ) ) ;
#8106 = VERTEX_POINT ( 'NONE', #14469 ) ;
#8107 = LINE ( 'NONE', #14731, #16468 ) ;
#8108 = ORIENTED_EDGE ( 'NONE', *, *, #12249, .F. ) ;
#8109 = EDGE_CURVE ( 'NONE', #4239, #10479, #1402, .T. ) ;
#8110 = DIRECTION ( 'NONE',  ( -0.000000000000000000, -1.000000000000000000, -0.000000000000000000 ) ) ;
#8111 = VECTOR ( 'NONE', #1811, 1000.000000000000000 ) ;
#8112 = ORIENTED_EDGE ( 'NONE', *, *, #15649, .T. ) ;
#8113 = ORIENTED_EDGE ( 'NONE', *, *, #6659, .T. ) ;
#8114 = DIRECTION ( 'NONE',  ( -0.7327934916262990317, -0.6804510993672779895, -8.333122608164345406E-17 ) ) ;
#8115 = CARTESIAN_POINT ( 'NONE',  ( -35.00000000000000000, 19.00000000000000000, -21.00000000000000000 ) ) ;
#8116 = CARTESIAN_POINT ( 'NONE',  ( 46.99999999999988631, 523.2161522479888163, -502.8936384967199729 ) ) ;
#8117 = VERTEX_POINT ( 'NONE', #7920 ) ;
#8118 = DIRECTION ( 'NONE',  ( -1.000000000000000000, -0.000000000000000000, -0.000000000000000000 ) ) ;
#8119 = DIRECTION ( 'NONE',  ( -0.000000000000000000, -1.000000000000000000, -0.000000000000000000 ) ) ;
#8120 = CIRCLE ( 'NONE', #2351, 14.59999999999999964 ) ;
#8121 = EDGE_CURVE ( 'NONE', #11164, #3748, #11162, .T. ) ;
#8122 = LINE ( 'NONE', #9249, #4941 ) ;
#8123 = AXIS2_PLACEMENT_3D ( 'NONE', #941, #16226, #4466 ) ;
#8124 = CARTESIAN_POINT ( 'NONE',  ( 394.0000000000001137, 339.1725919290087745, -9.945665743359786148 ) ) ;
#8125 = EDGE_CURVE ( 'NONE', #7313, #8452, #2611, .T. ) ;
#8126 = CYLINDRICAL_SURFACE ( 'NONE', #8415, 13.69540538389601991 ) ;
#8127 = FACE_OUTER_BOUND ( 'NONE', #11291, .T. ) ;
#8128 = CARTESIAN_POINT ( 'NONE',  ( -31.00000000000000000, 11.00000000000000000, -31.00000000000000000 ) ) ;
#8129 = LINE ( 'NONE', #7946, #14536 ) ;
#8131 = ORIENTED_EDGE ( 'NONE', *, *, #2037, .T. ) ;
#8130 = VERTEX_POINT ( 'NONE', #14547 ) ;
#8132 = EDGE_CURVE ( 'NONE', #1946, #6185, #5391, .T. ) ;
#8133 = CARTESIAN_POINT ( 'NONE',  ( 22.99999999999997513, 0.000000000000000000, 31.00000000000005684 ) ) ;
#8134 = VECTOR ( 'NONE', #2448, 1000.000000000000000 ) ;
#8135 = CARTESIAN_POINT ( 'NONE',  ( 0.7365999999999663927, 289.4957685731285437, 37.53315213583296384 ) ) ;
#8136 = CIRCLE ( 'NONE', #13900, 13.69540538389601991 ) ;
#8137 = CARTESIAN_POINT ( 'NONE',  ( -34.99999999999999289, 11.00000000000000000, -35.00000000000000711 ) ) ;
#8138 = CYLINDRICAL_SURFACE ( 'NONE', #7743, 6.473199999999998511 ) ;
#8139 = ORIENTED_EDGE ( 'NONE', *, *, #8558, .T. ) ;
#8140 = CARTESIAN_POINT ( 'NONE',  ( 10.00000000000000000, 425.7506394335853201, -11.00000000000000000 ) ) ;
#8141 = DIRECTION ( 'NONE',  ( 1.000000000000000000, 0.000000000000000000, 8.673617379884027583E-16 ) ) ;
#8143 = EDGE_CURVE ( 'NONE', #14371, #13400, #15833, .T. ) ;
#8142 = ORIENTED_EDGE ( 'NONE', *, *, #14119, .T. ) ;
#8144 = LINE ( 'NONE', #1794, #16963 ) ;
#8145 = LINE ( 'NONE', #8224, #12523 ) ;
#8146 = DIRECTION ( 'NONE',  ( 1.000000000000000000, -0.000000000000000000, 0.000000000000000000 ) ) ;
#8147 = AXIS2_PLACEMENT_3D ( 'NONE', #8725, #1860, #9843 ) ;
#8148 = ORIENTED_EDGE ( 'NONE', *, *, #897, .T. ) ;
#8149 = AXIS2_PLACEMENT_3D ( 'NONE', #6597, #11856, #15811 ) ;
#8150 = DIRECTION ( 'NONE',  ( -0.000000000000000000, -1.000000000000000000, 0.000000000000000000 ) ) ;
#8151 = CARTESIAN_POINT ( 'NONE',  ( -46.99999999999988631, 493.2350855268086320, -508.1801094700848580 ) ) ;
#8152 = DIRECTION ( 'NONE',  ( -1.000000000000000000, -0.000000000000000000, 0.000000000000000000 ) ) ;
#8153 = ORIENTED_EDGE ( 'NONE', *, *, #12318, .T. ) ;
#8154 = EDGE_CURVE ( 'NONE', #12451, #7744, #2377, .T. ) ;
#8155 = EDGE_CURVE ( 'NONE', #10824, #8801, #2954, .T. ) ;
#8156 = ADVANCED_FACE ( 'NONE', ( #9393 ), #6622, .F. ) ;
#8157 = CARTESIAN_POINT ( 'NONE',  ( -31.00000000000000000, 11.00000000000000000, -31.00000000000000000 ) ) ;
#8158 = ADVANCED_FACE ( 'NONE', ( #1583 ), #15744, .F. ) ;
#8159 = FACE_OUTER_BOUND ( 'NONE', #3039, .T. ) ;
#8160 = TOROIDAL_SURFACE ( 'NONE', #15564, 4.695405383895982609, 9.000000000000000000 ) ;
#8161 = ORIENTED_EDGE ( 'NONE', *, *, #5939, .T. ) ;
#8162 = CARTESIAN_POINT ( 'NONE',  ( -40.00000000000000711, 8.000000000000000000, -26.00000000000000000 ) ) ;
#8163 = DIRECTION ( 'NONE',  ( -0.000000000000000000, -1.000000000000000000, -0.000000000000000000 ) ) ;
#8164 = FACE_OUTER_BOUND ( 'NONE', #3342, .T. ) ;
#8165 = VERTEX_POINT ( 'NONE', #13266 ) ;
#8166 = DIRECTION ( 'NONE',  ( 0.000000000000000000, 0.000000000000000000, -1.000000000000000000 ) ) ;
#8167 = CARTESIAN_POINT ( 'NONE',  ( -54.99999999999999289, 515.4878487013597805, -546.7230258972048205 ) ) ;
#8168 = DIRECTION ( 'NONE',  ( -0.000000000000000000, 1.000000000000000000, -0.000000000000000000 ) ) ;
#8169 = EDGE_LOOP ( 'NONE', ( #13421, #14187, #8585, #7578 ) ) ;
#8170 = VERTEX_POINT ( 'NONE', #13177 ) ;
#8171 = ORIENTED_EDGE ( 'NONE', *, *, #11071, .F. ) ;
#8172 =( GEOMETRIC_REPRESENTATION_CONTEXT ( 3 ) GLOBAL_UNCERTAINTY_ASSIGNED_CONTEXT ( ( #183 ) ) GLOBAL_UNIT_ASSIGNED_CONTEXT ( ( #16217, #12355, #6842 ) ) REPRESENTATION_CONTEXT ( 'NONE', 'WORKASPACE' ) );
#8173 = CARTESIAN_POINT ( 'NONE',  ( -36.99999999999997868, 0.000000000000000000, -19.99999999999999289 ) ) ;
#8174 = ADVANCED_FACE ( 'NONE', ( #11885, #8188, #128, #10763, #6883, #5351 ), #5514, .F. ) ;
#8175 = ORIENTED_EDGE ( 'NONE', *, *, #6958, .T. ) ;
#8176 = APPLICATION_PROTOCOL_DEFINITION ( 'draft international standard', 'automotive_design', 1998, #2937 ) ;
#8177 = VERTEX_POINT ( 'NONE', #8005 ) ;
#8178 = VERTEX_POINT ( 'NONE', #1497 ) ;
#8179 = CARTESIAN_POINT ( 'NONE',  ( 40.00000000000000000, 0.000000000000000000, 26.00000000000000355 ) ) ;
#8180 = CARTESIAN_POINT ( 'NONE',  ( 75.00000000000000000, 0.000000000000000000, -7.000000000000006217 ) ) ;
#8181 = ORIENTED_EDGE ( 'NONE', *, *, #12153, .T. ) ;
#8182 = CARTESIAN_POINT ( 'NONE',  ( -3.000000000000000000, 41.00000000000000711, 9.013878188659973034 ) ) ;
#8183 = VECTOR ( 'NONE', #2175, 1000.000000000000000 ) ;
#8184 = DIRECTION ( 'NONE',  ( 0.000000000000000000, 1.000000000000000000, 0.000000000000000000 ) ) ;
#8185 = ORIENTED_EDGE ( 'NONE', *, *, #15158, .T. ) ;
#8186 = SURFACE_STYLE_FILL_AREA ( #9655 ) ;
#8187 = EDGE_LOOP ( 'NONE', ( #5781, #13897, #5443, #130 ) ) ;
#8188 = FACE_BOUND ( 'NONE', #1521, .T. ) ;
#8189 = CARTESIAN_POINT ( 'NONE',  ( -55.99999999999989342, 549.5810598491746077, -518.1154249974242703 ) ) ;
#8190 = ORIENTED_EDGE ( 'NONE', *, *, #2480, .T. ) ;
#8191 = PLANE ( 'NONE',  #1114 ) ;
#8192 = ORIENTED_EDGE ( 'NONE', *, *, #4380, .T. ) ;
#8193 = SHAPE_REPRESENTATION_RELATIONSHIP ( 'NONE' , 'NONE' ,  #2419, #3016 ) ;
#8194 = LINE ( 'NONE', #8375, #7014 ) ;
#8195 = CIRCLE ( 'NONE', #12851, 4.695405383896011919 ) ;
#8196 = ORIENTED_EDGE ( 'NONE', *, *, #10341, .F. ) ;
#8197 = ORIENTED_EDGE ( 'NONE', *, *, #4973, .F. ) ;
#8198 = DIRECTION ( 'NONE',  ( 0.000000000000000000, -0.000000000000000000, -1.000000000000000000 ) ) ;
#8199 = DIRECTION ( 'NONE',  ( -1.000000000000000000, 0.000000000000000000, -0.000000000000000000 ) ) ;
#8200 = DIRECTION ( 'NONE',  ( -1.000000000000000000, 0.000000000000000000, 0.000000000000000000 ) ) ;
#8201 = CARTESIAN_POINT ( 'NONE',  ( 394.0000000000001137, 339.4485271457189128, -10.62862937063367852 ) ) ;
#8202 = PLANE ( 'NONE',  #6671 ) ;
#8203 = LINE ( 'NONE', #4664, #4129 ) ;
#8204 = CARTESIAN_POINT ( 'NONE',  ( 40.00000000000000000, 68.00000000000000000, 26.00000000000000355 ) ) ;
#8205 = DIRECTION ( 'NONE',  ( -1.000000000000000000, -0.000000000000000000, -0.000000000000000000 ) ) ;
#8206 = DIRECTION ( 'NONE',  ( -0.000000000000000000, -1.000000000000000000, -0.000000000000000000 ) ) ;
#8207 = DIRECTION ( 'NONE',  ( 6.092845550116402428E-18, -0.9950371902099888199, 0.09950371902100227373 ) ) ;
#8208 = CARTESIAN_POINT ( 'NONE',  ( 394.0000000000001137, 240.7889724647196488, -10.68226574335980139 ) ) ;
#8210 = ORIENTED_EDGE ( 'NONE', *, *, #3625, .T. ) ;
#8209 = ORIENTED_EDGE ( 'NONE', *, *, #12571, .T. ) ;
#8211 = DIRECTION ( 'NONE',  ( 0.000000000000000000, -2.081668171172169746E-16, -1.000000000000000000 ) ) ;
#8212 = DIRECTION ( 'NONE',  ( 0.000000000000000000, 0.000000000000000000, 1.000000000000000000 ) ) ;
#8213 = EDGE_CURVE ( 'NONE', #13922, #4246, #6721, .T. ) ;
#8214 = EDGE_CURVE ( 'NONE', #11589, #15821, #5433, .T. ) ;
#8215 = DIRECTION ( 'NONE',  ( -2.920976200236483125E-16, 0.09950371902099772181, -0.9950371902099892640 ) ) ;
#8216 = CARTESIAN_POINT ( 'NONE',  ( 46.99999999999988631, 549.5810598491746077, -513.4200196135282113 ) ) ;
#8217 = VERTEX_POINT ( 'NONE', #1664 ) ;
#8218 = CARTESIAN_POINT ( 'NONE',  ( 30.99999999999999645, 68.00000000000000000, 31.00000000000001066 ) ) ;
#8219 = ADVANCED_FACE ( 'NONE', ( #12144 ), #6169, .F. ) ;
#8220 = AXIS2_PLACEMENT_3D ( 'NONE', #3678, #7682, #10534 ) ;
#8221 = LINE ( 'NONE', #13476, #1548 ) ;
#8222 = EDGE_LOOP ( 'NONE', ( #15513, #12194, #10836, #6966 ) ) ;
#8223 = PLANE ( 'NONE',  #13 ) ;
#8224 = CARTESIAN_POINT ( 'NONE',  ( -40.00000000000000000, 0.000000000000000000, -25.99999999999999645 ) ) ;
#8225 = CARTESIAN_POINT ( 'NONE',  ( -150.0000000000000000, 512.1906115401388888, -11.00000000000000000 ) ) ;
#8226 = LINE ( 'NONE', #13481, #2501 ) ;
#8227 = SURFACE_SIDE_STYLE ('',( #14850 ) ) ;
#8228 = DIRECTION ( 'NONE',  ( 0.000000000000000000, 0.000000000000000000, 1.000000000000000000 ) ) ;
#8229 = ORIENTED_EDGE ( 'NONE', *, *, #6139, .T. ) ;
#8230 = CARTESIAN_POINT ( 'NONE',  ( 55.99999999999989342, 549.5810598491749488, -575.3306267969850296 ) ) ;
#8231 = B_SPLINE_CURVE_WITH_KNOTS ( 'NONE', 3,
 ( #15326, #3562, #8799, #539, #711, #8438, #13928, #8694, #11253, #4721, #7378, #13600, #9814, #13678, #620, #16488, #9981, #4634 ),
 .UNSPECIFIED., .F., .F.,
 ( 4, 2, 2, 2, 2, 2, 2, 2, 4 ),
 ( 0.004721323624227211080, 0.005310725018217473184, 0.005900126412207735288, 0.006489527806197996525, 0.007078929200188269905, 0.007668330594178543284, 0.008257731988168816664, 0.008847133382159089177, 0.009436534776149363424 ),
 .UNSPECIFIED. ) ;
#8232 = VECTOR ( 'NONE', #16911, 1000.000000000000000 ) ;
#8233 = DIRECTION ( 'NONE',  ( 0.000000000000000000, 1.000000000000000000, 0.000000000000000000 ) ) ;
#8234 = ADVANCED_FACE ( 'NONE', ( #10941 ), #13104, .F. ) ;
#8235 = AXIS2_PLACEMENT_3D ( 'NONE', #14684, #166, #5388 ) ;
#8236 = DIRECTION ( 'NONE',  ( 0.000000000000000000, -0.9950371902099903743, -0.09950371902098545385 ) ) ;
#8237 = ORIENTED_EDGE ( 'NONE', *, *, #16609, .T. ) ;
#8238 = DIRECTION ( 'NONE',  ( -0.000000000000000000, 1.000000000000000000, -0.000000000000000000 ) ) ;
#8239 = PRODUCT ( 'Part8', 'Part8', '', ( #4323 ) ) ;
#8240 = UNCERTAINTY_MEASURE_WITH_UNIT (LENGTH_MEASURE( 1.000000000000000082E-05 ), #11087, 'distance_accuracy_value', 'NONE');
#8241 = EDGE_CURVE ( 'NONE', #10036, #1964, #3444, .T. ) ;
#8242 = LINE ( 'NONE', #11143, #13308 ) ;
#8243 = EDGE_CURVE ( 'NONE', #12863, #15101, #16654, .T. ) ;
#8244 = FACE_OUTER_BOUND ( 'NONE', #7636, .T. ) ;
#8245 = ORIENTED_EDGE ( 'NONE', *, *, #10938, .T. ) ;
#8246 = DIRECTION ( 'NONE',  ( 0.000000000000000000, 0.000000000000000000, -1.000000000000000000 ) ) ;
#8247 = EDGE_CURVE ( 'NONE', #16000, #8130, #14476, .T. ) ;
#8248 = CARTESIAN_POINT ( 'NONE',  ( 37.00000000000003553, -20.00000000000000000, 20.00000000000000000 ) ) ;
#8249 = DIRECTION ( 'NONE',  ( -0.000000000000000000, 0.9271838545667866471, 0.3746065934159141242 ) ) ;
#8250 = ORIENTED_EDGE ( 'NONE', *, *, #4342, .F. ) ;
#8251 = AXIS2_PLACEMENT_3D ( 'NONE', #3321, #15338, #11219 ) ;
#8252 =( NAMED_UNIT ( * ) SI_UNIT ( $, .STERADIAN. ) SOLID_ANGLE_UNIT ( ) );
#8253 = ORIENTED_EDGE ( 'NONE', *, *, #11827, .F. ) ;
#8254 = ORIENTED_EDGE ( 'NONE', *, *, #1199, .F. ) ;
#8255 = FACE_OUTER_BOUND ( 'NONE', #12839, .T. ) ;
#8256 = ORIENTED_EDGE ( 'NONE', *, *, #13911, .F. ) ;
#8257 = APPLICATION_PROTOCOL_DEFINITION ( 'draft international standard', 'automotive_design', 1998, #16199 ) ;
#8258 = VERTEX_POINT ( 'NONE', #14811 ) ;
#8259 = VECTOR ( 'NONE', #978, 1000.000000000000000 ) ;
#8260 = EDGE_LOOP ( 'NONE', ( #6728, #12642, #16676, #11953 ) ) ;
#8261 = DIRECTION ( 'NONE',  ( 6.123031769111888756E-17, 0.000000000000000000, 1.000000000000000000 ) ) ;
#8262 = EDGE_CURVE ( 'NONE', #12261, #10598, #3134, .T. ) ;
#8263 = LINE ( 'NONE', #1308, #15738 ) ;
#8264 = EDGE_LOOP ( 'NONE', ( #10326, #1793, #3747, #7728 ) ) ;
#8265 = CARTESIAN_POINT ( 'NONE',  ( 35.00000000000000711, 8.000000000000000000, -35.00000000000000711 ) ) ;
#8266 = EDGE_CURVE ( 'NONE', #13963, #10961, #4963, .T. ) ;
#8267 = CARTESIAN_POINT ( 'NONE',  ( 394.0000000000001137, 449.3157724647196005, -155.1251505852266632 ) ) ;
#8268 = EDGE_LOOP ( 'NONE', ( #14224, #11629 ) ) ;
#8269 = CARTESIAN_POINT ( 'NONE',  ( -26.00000000000000000, 19.00000000000000000, -40.00000000000000711 ) ) ;
#8270 = ORIENTED_EDGE ( 'NONE', *, *, #5777, .F. ) ;
#8271 = CARTESIAN_POINT ( 'NONE',  ( 10.00000000000000000, 309.2289037985890445, -150.1198051533984597 ) ) ;
#8272 = CARTESIAN_POINT ( 'NONE',  ( 0.000000000000000000, 239.4632308570078294, 86.73739990498292229 ) ) ;
#8273 = ORIENTED_EDGE ( 'NONE', *, *, #16025, .F. ) ;
#8274 = AXIS2_PLACEMENT_3D ( 'NONE', #7830, #2420, #11872 ) ;
#8275 = EDGE_LOOP ( 'NONE', ( #3770, #11151, #13822, #12836 ) ) ;
#8276 = DIRECTION ( 'NONE',  ( 0.000000000000000000, -1.000000000000000000, 0.000000000000000000 ) ) ;
#8277 = VECTOR ( 'NONE', #8057, 1000.000000000000000 ) ;
#8278 = PRESENTATION_LAYER_ASSIGNMENT (  '', '', ( #16497 ) ) ;
#8279 = ORIENTED_EDGE ( 'NONE', *, *, #1960, .F. ) ;
#8280 = ORIENTED_EDGE ( 'NONE', *, *, #9489, .F. ) ;
#8281 = DIRECTION ( 'NONE',  ( -0.000000000000000000, 0.000000000000000000, -1.000000000000000000 ) ) ;
#8282 = CARTESIAN_POINT ( 'NONE',  ( 0.000000000000000000, 10.00000000000000000, 0.000000000000000000 ) ) ;
#8283 = DIRECTION ( 'NONE',  ( 0.000000000000000000, 0.000000000000000000, 1.000000000000000000 ) ) ;
#8284 = VECTOR ( 'NONE', #6357, 1000.000000000000000 ) ;
#8285 = DIRECTION ( 'NONE',  ( 0.000000000000000000, -1.000000000000000000, 0.000000000000000000 ) ) ;
#8286 = DIRECTION ( 'NONE',  ( 0.000000000000000000, 1.000000000000000000, 0.000000000000000000 ) ) ;
#8287 = DIRECTION ( 'NONE',  ( 0.000000000000000000, 0.000000000000000000, -1.000000000000000000 ) ) ;
#8288 = AXIS2_PLACEMENT_3D ( 'NONE', #16633, #3334, #13809 ) ;
#8289 = CARTESIAN_POINT ( 'NONE',  ( -23.00000000000002132, 0.000000000000000000, 37.00000000000000711 ) ) ;
#8290 = CIRCLE ( 'NONE', #6082, 22.75209553982836397 ) ;
#8291 = DIRECTION ( 'NONE',  ( 0.000000000000000000, 0.000000000000000000, 1.000000000000000000 ) ) ;
#8292 = FACE_OUTER_BOUND ( 'NONE', #8260, .T. ) ;
#8293 = CARTESIAN_POINT ( 'NONE',  ( -55.99999999999989342, 493.2350855268086320, -508.1801094700848580 ) ) ;
#8294 = CARTESIAN_POINT ( 'NONE',  ( -31.81980515339462912, 0.000000000000000000, 31.81980515339465043 ) ) ;
#8296 = ORIENTED_EDGE ( 'NONE', *, *, #14431, .T. ) ;
#8295 = ORIENTED_EDGE ( 'NONE', *, *, #2445, .F. ) ;
#8297 = APPLICATION_CONTEXT ( 'automotive_design' ) ;
#8298 = AXIS2_PLACEMENT_3D ( 'NONE', #10565, #1552, #5667 ) ;
#8299 = FACE_OUTER_BOUND ( 'NONE', #11875, .T. ) ;
#8300 = EDGE_CURVE ( 'NONE', #8106, #5261, #14193, .T. ) ;
#8301 = CARTESIAN_POINT ( 'NONE',  ( -54.99999999999999289, 515.4878487013597805, -461.7230258972048205 ) ) ;
#8302 = CIRCLE ( 'NONE', #7458, 13.69540538389598083 ) ;
#8303 = CIRCLE ( 'NONE', #902, 5.000000000000000888 ) ;
#8304 = DIRECTION ( 'NONE',  ( 0.000000000000000000, 0.9950371902099903743, 0.09950371902098545385 ) ) ;
#8305 = DIRECTION ( 'NONE',  ( 0.000000000000000000, 0.000000000000000000, 1.000000000000000000 ) ) ;
#8306 = ORIENTED_EDGE ( 'NONE', *, *, #11710, .F. ) ;
#8307 = DIRECTION ( 'NONE',  ( 0.000000000000000000, 0.000000000000000000, -1.000000000000000000 ) ) ;
#8308 = AXIS2_PLACEMENT_3D ( 'NONE', #4369, #11451, #11277 ) ;
#8309 = LINE ( 'NONE', #12011, #8418 ) ;
#8310 = ORIENTED_EDGE ( 'NONE', *, *, #13151, .F. ) ;
#8311 = CARTESIAN_POINT ( 'NONE',  ( 5.941205806953520074, 0.000000000000000000, 0.000000000000000000 ) ) ;
#8312 = LINE ( 'NONE', #13315, #13898 ) ;
#8313 = CARTESIAN_POINT ( 'NONE',  ( -31.00000000000003197, 68.00000000000000000, -22.99999999999999645 ) ) ;
#8314 = AXIS2_PLACEMENT_3D ( 'NONE', #6719, #14809, #14724 ) ;
#8315 = PRODUCT_RELATED_PRODUCT_CATEGORY ( 'part', '', ( #4910 ) ) ;
#8316 = AXIS2_PLACEMENT_3D ( 'NONE', #8975, #11713, #7580 ) ;
#8317 = DIRECTION ( 'NONE',  ( 0.000000000000000000, 0.000000000000000000, -1.000000000000000000 ) ) ;
#8318 = AXIS2_PLACEMENT_3D ( 'NONE', #4857, #4608, #4772 ) ;
#8319 = PRESENTATION_STYLE_ASSIGNMENT (( #2821 ) ) ;
#8320 = LINE ( 'NONE', #13483, #16235 ) ;
#8321 = ORIENTED_EDGE ( 'NONE', *, *, #589, .F. ) ;
#8322 = CARTESIAN_POINT ( 'NONE',  ( -46.99999999999988631, 473.6663340069158039, -561.9448123979092315 ) ) ;
#8323 = CIRCLE ( 'NONE', #3933, 9.000000000000007105 ) ;
#8324 = EDGE_CURVE ( 'NONE', #4508, #12483, #765, .T. ) ;
#8325 = PLANE ( 'NONE',  #1355 ) ;
#8326 = LINE ( 'NONE', #5573, #16522 ) ;
#8327 = ORIENTED_EDGE ( 'NONE', *, *, #10761, .F. ) ;
#8328 = AXIS2_PLACEMENT_3D ( 'NONE', #8028, #8119, #13372 ) ;
#8329 = CIRCLE ( 'NONE', #929, 4.999999999999997335 ) ;
#8330 = DIRECTION ( 'NONE',  ( 1.000000000000000000, 0.000000000000000000, -0.000000000000000000 ) ) ;
#8331 = CARTESIAN_POINT ( 'NONE',  ( 45.00000000000000000, 493.2350855268086320, -521.8755148539809170 ) ) ;
#8332 = ORIENTED_EDGE ( 'NONE', *, *, #9845, .T. ) ;
#8333 = DIRECTION ( 'NONE',  ( 0.000000000000000000, 1.000000000000000000, 0.000000000000000000 ) ) ;
#8334 = DIRECTION ( 'NONE',  ( -1.000000000000000000, 0.000000000000000000, 0.000000000000000000 ) ) ;
#8335 = LINE ( 'NONE', #9461, #11683 ) ;
#8336 = VERTEX_POINT ( 'NONE', #4890 ) ;
#8337 = CONICAL_SURFACE ( 'NONE', #10526, 12.32407335584850117, 0.8899833664651138898 ) ;
#8338 = ADVANCED_FACE ( 'NONE', ( #8688 ), #12620, .F. ) ;
#8339 = SURFACE_STYLE_USAGE ( .BOTH. , #13836 ) ;
#8340 = EDGE_CURVE ( 'NONE', #3029, #1004, #3526, .T. ) ;
#8341 = EDGE_CURVE ( 'NONE', #3462, #3010, #13926, .T. ) ;
#8342 = ORIENTED_EDGE ( 'NONE', *, *, #9225, .F. ) ;
#8343 = ORIENTED_EDGE ( 'NONE', *, *, #6982, .F. ) ;
#8344 = COLOUR_RGB ( '', 0.40784314, 0.44705882, 0.49803922) ;
#8345 = DIRECTION ( 'NONE',  ( 0.000000000000000000, 0.000000000000000000, 1.000000000000000000 ) ) ;
#8346 =( GEOMETRIC_REPRESENTATION_CONTEXT ( 3 ) GLOBAL_UNCERTAINTY_ASSIGNED_CONTEXT ( ( #2744 ) ) GLOBAL_UNIT_ASSIGNED_CONTEXT ( ( #7740, #10340, #9046 ) ) REPRESENTATION_CONTEXT ( 'NONE', 'WORKASPACE' ) );
#8347 = AXIS2_PLACEMENT_3D ( 'NONE', #3206, #3284, #2073 ) ;
#8348 = VERTEX_POINT ( 'NONE', #10135 ) ;
#8349 = ADVANCED_FACE ( 'NONE', ( #12799 ), #7293, .T. ) ;
#8350 = DIRECTION ( 'NONE',  ( 0.000000000000000000, 0.000000000000000000, 1.000000000000000000 ) ) ;
#8351 = ADVANCED_FACE ( 'NONE', ( #1756 ), #11331, .F. ) ;
#8352 = EDGE_CURVE ( 'NONE', #10374, #1948, #8369, .T. ) ;
#8353 = AXIS2_PLACEMENT_3D ( 'NONE', #16793, #16634, #11311 ) ;
#8354 = ORIENTED_EDGE ( 'NONE', *, *, #11799, .T. ) ;
#8355 = MANIFOLD_SOLID_BREP ( 'Imported1', #7155 ) ;
#8356 = CARTESIAN_POINT ( 'NONE',  ( 55.99999999999989342, 473.6663340069157471, -531.5012393965008641 ) ) ;
#8357 = ORIENTED_EDGE ( 'NONE', *, *, #9390, .T. ) ;
#8358 = CARTESIAN_POINT ( 'NONE',  ( 25.99999999999999645, 11.00000000000000000, 40.00000000000000711 ) ) ;
#8359 = FACE_OUTER_BOUND ( 'NONE', #8818, .T. ) ;
#8360 = ORIENTED_EDGE ( 'NONE', *, *, #15708, .T. ) ;
#8361 = DIRECTION ( 'NONE',  ( 0.000000000000000000, -1.000000000000000000, 0.000000000000000000 ) ) ;
#8362 = AXIS2_PLACEMENT_3D ( 'NONE', #3538, #14010, #8776 ) ;
#8363 = LINE ( 'NONE', #13608, #13359 ) ;
#8364 = ORIENTED_EDGE ( 'NONE', *, *, #16233, .T. ) ;
#8365 = EDGE_CURVE ( 'NONE', #14475, #12430, #16172, .T. ) ;
#8366 = VECTOR ( 'NONE', #11582, 1000.000000000000000 ) ;
#8367 = LINE ( 'NONE', #15999, #15711 ) ;
#8368 = ORIENTED_EDGE ( 'NONE', *, *, #5861, .F. ) ;
#8369 = LINE ( 'NONE', #7451, #5400 ) ;
#8370 = PLANE ( 'NONE',  #645 ) ;
#8371 = EDGE_LOOP ( 'NONE', ( #13432, #4436, #16455, #13103 ) ) ;
#8372 = ORIENTED_EDGE ( 'NONE', *, *, #2555, .F. ) ;
#8373 = ADVANCED_FACE ( 'NONE', ( #7880 ), #85, .T. ) ;
#8374 = EDGE_CURVE ( 'NONE', #15631, #13257, #15455, .T. ) ;
#8375 = CARTESIAN_POINT ( 'NONE',  ( -25.99999999999999645, 68.00000000000000000, -31.00000000000003197 ) ) ;
#8376 = ADVANCED_FACE ( 'NONE', ( #6497 ), #11933, .T. ) ;
#8377 = CYLINDRICAL_SURFACE ( 'NONE', #729, 2.999999999999995559 ) ;
#8378 = ADVANCED_FACE ( 'NONE', ( #15545 ), #4033, .F. ) ;
#8379 = ORIENTED_EDGE ( 'NONE', *, *, #1228, .F. ) ;
#8380 = ORIENTED_EDGE ( 'NONE', *, *, #4766, .F. ) ;
#8381 = LINE ( 'NONE', #7065, #9680 ) ;
#8382 = VECTOR ( 'NONE', #10721, 1000.000000000000000 ) ;
#8383 = VECTOR ( 'NONE', #11149, 1000.000000000000000 ) ;
#8384 = DIRECTION ( 'NONE',  ( -0.8502651466878615727, -0.5263546146162958461, -6.445984940062853155E-17 ) ) ;
#8385 = DIRECTION ( 'NONE',  ( -1.000000000000000000, -0.000000000000000000, -0.000000000000000000 ) ) ;
#8386 = CARTESIAN_POINT ( 'NONE',  ( 46.99999999999988631, 473.6663340069157471, -517.8058340126048051 ) ) ;
#8387 = PRODUCT_DEFINITION_SHAPE ( 'NONE', 'NONE',  #16983 ) ;
#8388 = CARTESIAN_POINT ( 'NONE',  ( -45.00000000000000000, 473.6663340069158039, -561.9448123979092315 ) ) ;
#8389 = FACE_OUTER_BOUND ( 'NONE', #12356, .T. ) ;
#8390 = DIRECTION ( 'NONE',  ( 0.000000000000000000, 0.000000000000000000, 1.000000000000000000 ) ) ;
#8391 = CARTESIAN_POINT ( 'NONE',  ( 31.00000000000003553, 10.00000000000000000, -22.99999999999999645 ) ) ;
#8392 = CARTESIAN_POINT ( 'NONE',  ( 30.99999999999997868, 0.000000000000000000, -30.99999999999999645 ) ) ;
#8393 = VECTOR ( 'NONE', #14065, 1000.000000000000000 ) ;
#8394 = LINE ( 'NONE', #12502, #9995 ) ;
#8395 = DIRECTION ( 'NONE',  ( 0.000000000000000000, 0.000000000000000000, 1.000000000000000000 ) ) ;
#8397 = ORIENTED_EDGE ( 'NONE', *, *, #4488, .T. ) ;
#8396 = ORIENTED_EDGE ( 'NONE', *, *, #15755, .T. ) ;
#8398 = CARTESIAN_POINT ( 'NONE',  ( 0.7808854937525596673, 38.09666348058623697, 9.469847369592788056 ) ) ;
#8399 = EDGE_CURVE ( 'NONE', #11, #12507, #6412, .T. ) ;
#8400 = LINE ( 'NONE', #16375, #11565 ) ;
#8401 = DIRECTION ( 'NONE',  ( 0.000000000000000000, 1.000000000000000000, 0.000000000000000000 ) ) ;
#8402 = DIRECTION ( 'NONE',  ( 0.000000000000000000, 1.000000000000000000, 0.000000000000000000 ) ) ;
#8403 = AXIS2_PLACEMENT_3D ( 'NONE', #3102, #357, #9549 ) ;
#8404 = EDGE_LOOP ( 'NONE', ( #7345, #7723, #7307, #4050 ) ) ;
#8405 = CIRCLE ( 'NONE', #10587, 13.69540538389601991 ) ;
#8406 = DIRECTION ( 'NONE',  ( 0.000000000000000000, 1.000000000000000000, 0.000000000000000000 ) ) ;
#8407 = EDGE_LOOP ( 'NONE', ( #5023, #3898 ) ) ;
#8408 = FACE_OUTER_BOUND ( 'NONE', #8275, .T. ) ;
#8409 = EDGE_CURVE ( 'NONE', #11373, #4234, #3696, .T. ) ;
#8410 = CARTESIAN_POINT ( 'NONE',  ( -3.302699999998768288, 193.4898140233617880, 37.52989836422148073 ) ) ;
#8411 = DIRECTION ( 'NONE',  ( 0.000000000000000000, 0.000000000000000000, -1.000000000000000000 ) ) ;
#8412 = FACE_OUTER_BOUND ( 'NONE', #8596, .T. ) ;
#8413 = FILL_AREA_STYLE ('',( #9351 ) ) ;
#8414 = VERTEX_POINT ( 'NONE', #14175 ) ;
#8415 = AXIS2_PLACEMENT_3D ( 'NONE', #11906, #1517, #8291 ) ;
#8416 = EDGE_CURVE ( 'NONE', #4278, #3029, #4054, .T. ) ;
#8417 = DIRECTION ( 'NONE',  ( 0.000000000000000000, 0.000000000000000000, -1.000000000000000000 ) ) ;
#8418 = VECTOR ( 'NONE', #4105, 1000.000000000000000 ) ;
#8419 = CARTESIAN_POINT ( 'NONE',  ( -34.99999999999999289, 11.00000000000000000, 35.00000000000000711 ) ) ;
#8420 = DIRECTION ( 'NONE',  ( 0.000000000000000000, 0.000000000000000000, 1.000000000000000000 ) ) ;
#8421 = ORIENTED_EDGE ( 'NONE', *, *, #13720, .T. ) ;
#8422 = CARTESIAN_POINT ( 'NONE',  ( 4.549999999999999822, 0.000000000000000000, -14.27500000000000036 ) ) ;
#8423 = VECTOR ( 'NONE', #10011, 1000.000000000000000 ) ;
#8424 = DIRECTION ( 'NONE',  ( 0.000000000000000000, -1.000000000000000000, -0.000000000000000000 ) ) ;
#8425 = ORIENTED_EDGE ( 'NONE', *, *, #12331, .F. ) ;
#8426 = AXIS2_PLACEMENT_3D ( 'NONE', #210, #1315, #30 ) ;
#8427 = DIRECTION ( 'NONE',  ( -0.000000000000000000, -1.000000000000000000, -0.000000000000000000 ) ) ;
#8428 = FACE_OUTER_BOUND ( 'NONE', #7111, .T. ) ;
#8429 = LINE ( 'NONE', #16231, #9503 ) ;
#8430 = ORIENTED_EDGE ( 'NONE', *, *, #2898, .F. ) ;
#8431 = FILL_AREA_STYLE ('',( #8687 ) ) ;
#8432 = ORIENTED_EDGE ( 'NONE', *, *, #9315, .F. ) ;
#8433 = ORIENTED_EDGE ( 'NONE', *, *, #14884, .T. ) ;
#8434 = DIRECTION ( 'NONE',  ( 0.000000000000000000, 0.000000000000000000, -1.000000000000000000 ) ) ;
#8435 = APPLICATION_PROTOCOL_DEFINITION ( 'draft international standard', 'automotive_design', 1998, #11474 ) ;
#8436 = AXIS2_PLACEMENT_3D ( 'NONE', #4150, #5611, #2691 ) ;
#8437 = ORIENTED_EDGE ( 'NONE', *, *, #7672, .F. ) ;
#8438 = CARTESIAN_POINT ( 'NONE',  ( 1.334572366541260990, 62.69404904380762389, 9.407584458684453921 ) ) ;
#8439 = ORIENTED_EDGE ( 'NONE', *, *, #8546, .F. ) ;
#8440 = ADVANCED_FACE ( 'NONE', ( #5305 ), #7624, .F. ) ;
#8441 = LINE ( 'NONE', #10069, #3348 ) ;
#8442 = DIRECTION ( 'NONE',  ( 1.000000000000000000, 0.000000000000000000, 0.000000000000000000 ) ) ;
#8443 = VERTEX_POINT ( 'NONE', #1111 ) ;
#8444 = PLANE ( 'NONE',  #7203 ) ;
#8445 = DIRECTION ( 'NONE',  ( 0.000000000000000000, 0.000000000000000000, -1.000000000000000000 ) ) ;
#8446 = ORIENTED_EDGE ( 'NONE', *, *, #8340, .T. ) ;
#8447 = AXIS2_PLACEMENT_3D ( 'NONE', #4715, #8763, #16482 ) ;
#8448 = EDGE_CURVE ( 'NONE', #10067, #11352, #2565, .T. ) ;
#8449 = VERTEX_POINT ( 'NONE', #5053 ) ;
#8450 = CARTESIAN_POINT ( 'NONE',  ( 5.945602903476760126, 0.000000000000000000, 0.000000000000000000 ) ) ;
#8451 = ORIENTED_EDGE ( 'NONE', *, *, #8409, .T. ) ;
#8452 = VERTEX_POINT ( 'NONE', #9095 ) ;
#8453 = ORIENTED_EDGE ( 'NONE', *, *, #6847, .T. ) ;
#8454 = ORIENTED_EDGE ( 'NONE', *, *, #1688, .T. ) ;
#8455 = CARTESIAN_POINT ( 'NONE',  ( -0.1969510947806061563, 38.00000000000000711, 9.500000000000003553 ) ) ;
#8456 = EDGE_CURVE ( 'NONE', #16882, #12691, #6227, .T. ) ;
#8457 = VECTOR ( 'NONE', #16762, 1000.000000000000000 ) ;
#8458 = DIRECTION ( 'NONE',  ( -1.000000000000000000, 0.000000000000000000, 0.000000000000000000 ) ) ;
#8459 = DIRECTION ( 'NONE',  ( 0.9998870921963913805, 0.01502673813723916056, 0.000000000000000000 ) ) ;
#8460 = DIRECTION ( 'NONE',  ( -1.000000000000000000, -0.000000000000000000, -0.000000000000000000 ) ) ;
#8461 = FACE_OUTER_BOUND ( 'NONE', #7657, .T. ) ;
#8462 = ADVANCED_FACE ( 'NONE', ( #7792 ), #13053, .F. ) ;
#8463 = ADVANCED_FACE ( 'NONE', ( #5213 ), #13382, .T. ) ;
#8464 = EDGE_CURVE ( 'NONE', #11320, #14998, #15840, .T. ) ;
#8465 = PLANE ( 'NONE',  #10952 ) ;
#8466 = ADVANCED_FACE ( 'NONE', ( #14770 ), #8160, .T. ) ;
#8467 = CARTESIAN_POINT ( 'NONE',  ( -3.270000000000000462, 264.4632308570090231, 287.5298983642207986 ) ) ;
#8468 = VERTEX_POINT ( 'NONE', #2997 ) ;
#8469 = CARTESIAN_POINT ( 'NONE',  ( 3.500000000000000000, 0.000000000000000000, 0.000000000000000000 ) ) ;
#8470 = DIRECTION ( 'NONE',  ( 0.000000000000000000, 0.000000000000000000, -1.000000000000000000 ) ) ;
#8471 = PLANE ( 'NONE',  #2296 ) ;
#8472 = AXIS2_PLACEMENT_3D ( 'NONE', #1599, #1859, #1777 ) ;
#8473 = FACE_BOUND ( 'NONE', #16772, .T. ) ;
#8475 = EDGE_LOOP ( 'NONE', ( #16138, #16326 ) ) ;
#8474 = VERTEX_POINT ( 'NONE', #12100 ) ;
#8476 = CARTESIAN_POINT ( 'NONE',  ( 449.9999999999998295, 104.2500000000000142, 0.000000000000000000 ) ) ;
#8477 = ITEM_DEFINED_TRANSFORMATION ( 'NONE', 'NONE', #7502,  #1488 ) ;
#8478 = CARTESIAN_POINT ( 'NONE',  ( -55.99999999999989342, 493.2350855268092573, -585.2659423243250103 ) ) ;
#8479 = CARTESIAN_POINT ( 'NONE',  ( 19.99999999999995381, 0.000000000000000000, -39.99999999999999289 ) ) ;
#8480 = CARTESIAN_POINT ( 'NONE',  ( 56.73000000000001108, 217.7170024689955596, 287.2045212030222388 ) ) ;
#8481 = ORIENTED_EDGE ( 'NONE', *, *, #16059, .T. ) ;
#8482 = AXIS2_PLACEMENT_3D ( 'NONE', #15071, #15151, #3308 ) ;
#8483 = EDGE_CURVE ( 'NONE', #594, #4006, #255, .T. ) ;
#8484 = CARTESIAN_POINT ( 'NONE',  ( -46.99999999999988631, 493.2350855268092573, -598.9613477082210693 ) ) ;
#8485 = ORIENTED_EDGE ( 'NONE', *, *, #14517, .T. ) ;
#8486 = CARTESIAN_POINT ( 'NONE',  ( 394.0000000000001137, 339.1725919290087745, -16.41886574335978821 ) ) ;
#8487 = EDGE_CURVE ( 'NONE', #1995, #13331, #12296, .T. ) ;
#8488 = CARTESIAN_POINT ( 'NONE',  ( -0.3121190734725042826, 189.5736389302157647, 37.58596727633950252 ) ) ;
#8489 = CARTESIAN_POINT ( 'NONE',  ( 30.99999999999997868, 10.00000000000000000, -30.99999999999999645 ) ) ;
#8490 = CIRCLE ( 'NONE', #7130, 36.50000000000000000 ) ;
#8491 = CARTESIAN_POINT ( 'NONE',  ( 0.000000000000000000, 240.7889724647196488, -110.6822657433598067 ) ) ;
#8492 = DIRECTION ( 'NONE',  ( 0.000000000000000000, 0.000000000000000000, 1.000000000000000000 ) ) ;
#8493 = MANIFOLD_SOLID_BREP ( 'Cut-Extrude1', #13760 ) ;
#8494 = ORIENTED_EDGE ( 'NONE', *, *, #12830, .T. ) ;
#8495 = DIRECTION ( 'NONE',  ( 0.000000000000000000, 0.000000000000000000, 1.000000000000000000 ) ) ;
#8496 = LINE ( 'NONE', #3180, #9319 ) ;
#8497 = ADVANCED_FACE ( 'NONE', ( #9704 ), #4874, .T. ) ;
#8498 = AXIS2_PLACEMENT_3D ( 'NONE', #13575, #9619, #7025 ) ;
#8499 = ORIENTED_EDGE ( 'NONE', *, *, #1916, .T. ) ;
#8500 = CARTESIAN_POINT ( 'NONE',  ( 30.99999999999995737, 0.000000000000000000, 31.00000000000000000 ) ) ;
#8501 = DIRECTION ( 'NONE',  ( 0.000000000000000000, 0.000000000000000000, 1.000000000000000000 ) ) ;
#8502 = ORIENTED_EDGE ( 'NONE', *, *, #9518, .F. ) ;
#8503 = LINE ( 'NONE', #12704, #2852 ) ;
#8504 = CARTESIAN_POINT ( 'NONE',  ( 55.99999999999989342, 493.2350855268086320, -508.1801094700848580 ) ) ;
#8505 = DIRECTION ( 'NONE',  ( 1.000000000000000000, 0.000000000000000000, 0.000000000000000000 ) ) ;
#8506 = ORIENTED_EDGE ( 'NONE', *, *, #14147, .F. ) ;
#8507 = ORIENTED_EDGE ( 'NONE', *, *, #11444, .F. ) ;
#8508 = ORIENTED_EDGE ( 'NONE', *, *, #10392, .F. ) ;
#8509 = AXIS2_PLACEMENT_3D ( 'NONE', #7412, #8395, #16526 ) ;
#8510 = FACE_OUTER_BOUND ( 'NONE', #8945, .T. ) ;
#8511 = CIRCLE ( 'NONE', #9306, 84.99999999999997158 ) ;
#8512 = APPLICATION_PROTOCOL_DEFINITION ( 'draft international standard', 'automotive_design', 1998, #7082 ) ;
#8513 =( LENGTH_UNIT ( ) NAMED_UNIT ( * ) SI_UNIT ( .MILLI., .METRE. ) );
#8514 = MANIFOLD_SOLID_BREP ( 'Cut-Extrude3', #1138 ) ;
#8515 = DIRECTION ( 'NONE',  ( -0.000000000000000000, -1.000000000000000000, -0.000000000000000000 ) ) ;
#8516 = ORIENTED_EDGE ( 'NONE', *, *, #194, .T. ) ;
#8517 = FACE_OUTER_BOUND ( 'NONE', #2104, .T. ) ;
#8518 = DIRECTION ( 'NONE',  ( 0.000000000000000000, 0.000000000000000000, -1.000000000000000000 ) ) ;
#8519 = VECTOR ( 'NONE', #3744, 1000.000000000000000 ) ;
#8520 = VERTEX_POINT ( 'NONE', #2914 ) ;
#8522 = DIRECTION ( 'NONE',  ( 1.000000000000000000, 0.000000000000000000, 0.000000000000000000 ) ) ;
#8521 = VECTOR ( 'NONE', #16608, 1000.000000000000000 ) ;
#8523 = CARTESIAN_POINT ( 'NONE',  ( -3.270000000000000462, 189.4851275752425295, -18.94851275752489883 ) ) ;
#8524 = ORIENTED_EDGE ( 'NONE', *, *, #10123, .F. ) ;
#8525 = CARTESIAN_POINT ( 'NONE',  ( 415.3629108289414944, 306.8565854934392974, -6.736600000000000144 ) ) ;
#8526 = ORIENTED_EDGE ( 'NONE', *, *, #16123, .T. ) ;
#8527 = VERTEX_POINT ( 'NONE', #13403 ) ;
#8528 = EDGE_CURVE ( 'NONE', #1641, #386, #13940, .T. ) ;
#8529 = EDGE_CURVE ( 'NONE', #1142, #8018, #16053, .T. ) ;
#8530 = ORIENTED_EDGE ( 'NONE', *, *, #15951, .F. ) ;
#8531 = AXIS2_PLACEMENT_3D ( 'NONE', #14758, #8215, #12267 ) ;
#8532 = EDGE_LOOP ( 'NONE', ( #14264, #8078, #1650, #2513 ) ) ;
#8533 = ADVANCED_FACE ( 'NONE', ( #13733 ), #2293, .T. ) ;
#8534 = ORIENTED_EDGE ( 'NONE', *, *, #808, .F. ) ;
#8535 = PLANE ( 'NONE',  #15424 ) ;
#8536 = DIRECTION ( 'NONE',  ( 1.000000000000000000, -0.000000000000000000, 0.000000000000000000 ) ) ;
#8537 = DIRECTION ( 'NONE',  ( 0.000000000000000000, -0.9950371902099890420, 0.09950371902099952592 ) ) ;
#8538 = DIRECTION ( 'NONE',  ( 0.000000000000000000, 0.000000000000000000, 1.000000000000000000 ) ) ;
#8539 = LINE ( 'NONE', #13779, #13555 ) ;
#8540 = CIRCLE ( 'NONE', #4961, 9.999999999999994671 ) ;
#8541 = DIRECTION ( 'NONE',  ( 0.000000000000000000, 0.000000000000000000, 1.000000000000000000 ) ) ;
#8542 = CARTESIAN_POINT ( 'NONE',  ( -20.99999999999999645, 8.000000000000000000, -31.00000000000003553 ) ) ;
#8543 = ORIENTED_EDGE ( 'NONE', *, *, #1322, .F. ) ;
#8544 = DIRECTION ( 'NONE',  ( -1.000000000000000000, -0.000000000000000000, -0.000000000000000000 ) ) ;
#8545 = PLANE ( 'NONE',  #2259 ) ;
#8546 = EDGE_CURVE ( 'NONE', #4127, #5865, #3336, .T. ) ;
#8547 = CIRCLE ( 'NONE', #15124, 18.50000000000000000 ) ;
#8548 = CLOSED_SHELL ( 'NONE', ( #3715, #2357, #7084, #13451, #9540, #7609 ) ) ;
#8549 = DIRECTION ( 'NONE',  ( 0.000000000000000000, 0.000000000000000000, -1.000000000000000000 ) ) ;
#8550 = CIRCLE ( 'NONE', #7994, 13.69540538389601991 ) ;
#8551 = EDGE_CURVE ( 'NONE', #4736, #10866, #5909, .T. ) ;
#8552 = CARTESIAN_POINT ( 'NONE',  ( 54.99999999999999289, 515.4878487013597805, -546.7230258972048205 ) ) ;
#8554 = ORIENTED_EDGE ( 'NONE', *, *, #2225, .F. ) ;
#8553 = ORIENTED_EDGE ( 'NONE', *, *, #6232, .F. ) ;
#8555 = DIRECTION ( 'NONE',  ( 0.000000000000000000, 0.000000000000000000, -1.000000000000000000 ) ) ;
#8556 = ORIENTED_EDGE ( 'NONE', *, *, #16642, .F. ) ;
#8557 = ADVANCED_BREP_SHAPE_REPRESENTATION ( '', ( #8493, #1488 ), #2021 ) ;
#8558 = EDGE_CURVE ( 'NONE', #1379, #14282, #3505, .T. ) ;
#8559 = EDGE_CURVE ( 'NONE', #14542, #221, #11401, .T. ) ;
#8560 = DIRECTION ( 'NONE',  ( -1.000000000000000000, -0.000000000000000000, -0.000000000000000000 ) ) ;
#8561 = EDGE_CURVE ( 'NONE', #9920, #16153, #6063, .T. ) ;
#8562 = EDGE_CURVE ( 'NONE', #2916, #11402, #11185, .T. ) ;
#8563 = FACE_OUTER_BOUND ( 'NONE', #2567, .T. ) ;
#8564 = CARTESIAN_POINT ( 'NONE',  ( 25.99999999999996092, 3.000000000000000000, -31.00000000000003197 ) ) ;
#8565 = ORIENTED_EDGE ( 'NONE', *, *, #2060, .F. ) ;
#8566 = AXIS2_PLACEMENT_3D ( 'NONE', #6471, #9247, #5183 ) ;
#8567 = VECTOR ( 'NONE', #9948, 1000.000000000000000 ) ;
#8568 = STYLED_ITEM ( 'NONE', ( #10867 ), #14168 ) ;
#8569 = FACE_OUTER_BOUND ( 'NONE', #5091, .T. ) ;
#8570 = CARTESIAN_POINT ( 'NONE',  ( 3.850000000000000089, 14.27500000000000036, 0.000000000000000000 ) ) ;
#8571 = ORIENTED_EDGE ( 'NONE', *, *, #193, .T. ) ;
#8572 = CARTESIAN_POINT ( 'NONE',  ( -35.00000000000000000, 19.00000000000000000, -21.00000000000000000 ) ) ;
#8573 = CARTESIAN_POINT ( 'NONE',  ( 0.000000000000000000, 66.00000000000000000, 0.000000000000000000 ) ) ;
#8574 = CARTESIAN_POINT ( 'NONE',  ( -37.00000000000000711, 10.00000000000000000, -23.00000000000000000 ) ) ;
#8575 = DIRECTION ( 'NONE',  ( 1.000000000000000000, 0.000000000000000000, 0.000000000000000000 ) ) ;
#8576 = CARTESIAN_POINT ( 'NONE',  ( 55.99999999999989342, 549.5810598491749488, -575.3306267969850296 ) ) ;
#8577 = ORIENTED_EDGE ( 'NONE', *, *, #1292, .F. ) ;
#8578 = CARTESIAN_POINT ( 'NONE',  ( -25.99999999999999645, 0.000000000000000000, -39.99999999999999289 ) ) ;
#8579 = VECTOR ( 'NONE', #9588, 1000.000000000000000 ) ;
#8580 = AXIS2_PLACEMENT_3D ( 'NONE', #11411, #16644, #6236 ) ;
#8581 = EDGE_CURVE ( 'NONE', #15297, #15749, #507, .T. ) ;
#8582 = EDGE_CURVE ( 'NONE', #7385, #8170, #16388, .T. ) ;
#8583 = CYLINDRICAL_SURFACE ( 'NONE', #3821, 13.69540538389601991 ) ;
#8584 = ADVANCED_FACE ( 'NONE', ( #7269 ), #4693, .T. ) ;
#8585 = ORIENTED_EDGE ( 'NONE', *, *, #7120, .T. ) ;
#8586 = AXIS2_PLACEMENT_3D ( 'NONE', #2212, #12948, #6402 ) ;
#8587 = ORIENTED_EDGE ( 'NONE', *, *, #16542, .F. ) ;
#8588 = DIRECTION ( 'NONE',  ( 0.000000000000000000, -1.000000000000000000, 0.000000000000000000 ) ) ;
#8589 = PLANE ( 'NONE',  #4831 ) ;
#8590 = ORIENTED_EDGE ( 'NONE', *, *, #4264, .T. ) ;
#8591 = DIRECTION ( 'NONE',  ( 0.000000000000000000, 0.000000000000000000, 1.000000000000000000 ) ) ;
#8592 = VECTOR ( 'NONE', #14380, 1000.000000000000114 ) ;
#8593 = AXIS2_PLACEMENT_3D ( 'NONE', #14243, #2461, #16888 ) ;
#8594 = CARTESIAN_POINT ( 'NONE',  ( 10.00000000000000000, 372.8685141053778693, -79.88019484660868841 ) ) ;
#8595 = DIRECTION ( 'NONE',  ( 1.000000000000000000, 0.000000000000000000, 0.000000000000000000 ) ) ;
#8596 = EDGE_LOOP ( 'NONE', ( #12497, #11445 ) ) ;
#8597 = CARTESIAN_POINT ( 'NONE',  ( -26.00000000000002842, 3.000000000000000000, 31.00000000000003908 ) ) ;
#8598 = ORIENTED_EDGE ( 'NONE', *, *, #8653, .F. ) ;
#8599 = ORIENTED_EDGE ( 'NONE', *, *, #10862, .T. ) ;
#8600 = VECTOR ( 'NONE', #1490, 1000.000000000000000 ) ;
#8601 = CARTESIAN_POINT ( 'NONE',  ( -31.00000000000005684, 68.00000000000000000, 23.00000000000000355 ) ) ;
#8602 = VECTOR ( 'NONE', #5248, 1000.000000000000000 ) ;
#8603 = CIRCLE ( 'NONE', #9978, 9.500000000000000000 ) ;
#8604 =( NAMED_UNIT ( * ) SI_UNIT ( $, .STERADIAN. ) SOLID_ANGLE_UNIT ( ) );
#8605 = VECTOR ( 'NONE', #11297, 1000.000000000000000 ) ;
#8606 = DIRECTION ( 'NONE',  ( 0.000000000000000000, 0.000000000000000000, -1.000000000000000000 ) ) ;
#8607 = ORIENTED_EDGE ( 'NONE', *, *, #9636, .T. ) ;
#8608 = FACE_OUTER_BOUND ( 'NONE', #5259, .T. ) ;
#8609 = LINE ( 'NONE', #3123, #2301 ) ;
#8610 = AXIS2_PLACEMENT_3D ( 'NONE', #5673, #14699, #2748 ) ;
#8611 = ORIENTED_EDGE ( 'NONE', *, *, #8882, .F. ) ;
#8612 = LINE ( 'NONE', #5943, #1761 ) ;
#8613 = LINE ( 'NONE', #15226, #11708 ) ;
#8614 = ORIENTED_EDGE ( 'NONE', *, *, #7089, .F. ) ;
#8615 = AXIS2_PLACEMENT_3D ( 'NONE', #13075, #15637, #3875 ) ;
#8616 = DIRECTION ( 'NONE',  ( 0.000000000000000000, 0.000000000000000000, -1.000000000000000000 ) ) ;
#8617 = CIRCLE ( 'NONE', #7757, 59.99999999999994316 ) ;
#8618 = ADVANCED_FACE ( 'NONE', ( #11066 ), #4869, .T. ) ;
#8619 = ORIENTED_EDGE ( 'NONE', *, *, #7702, .T. ) ;
#8620 = ORIENTED_EDGE ( 'NONE', *, *, #15067, .T. ) ;
#8621 = VECTOR ( 'NONE', #9683, 1000.000000000000000 ) ;
#8622 = ORIENTED_EDGE ( 'NONE', *, *, #689, .F. ) ;
#8623 = AXIS2_PLACEMENT_3D ( 'NONE', #13665, #15107, #7193 ) ;
#8624 = EDGE_CURVE ( 'NONE', #11329, #12451, #7430, .T. ) ;
#8625 = VERTEX_POINT ( 'NONE', #5820 ) ;
#8626 = MECHANICAL_DESIGN_GEOMETRIC_PRESENTATION_REPRESENTATION (  '', ( #11632 ), #16833 ) ;
#8627 = EDGE_LOOP ( 'NONE', ( #9042, #11262 ) ) ;
#8629 = CARTESIAN_POINT ( 'NONE',  ( 1.399999999999999911, 15.25000000000000000, 0.000000000000000000 ) ) ;
#8628 = AXIS2_PLACEMENT_3D ( 'NONE', #15485, #9218, #3721 ) ;
#8630 = AXIS2_PLACEMENT_3D ( 'NONE', #9817, #15122, #12304 ) ;
#8631 = CARTESIAN_POINT ( 'NONE',  ( -39.99999999999997868, 3.000000000000000000, 26.00000000000000355 ) ) ;
#8632 = CARTESIAN_POINT ( 'NONE',  ( -13.11912225705329327, 2.755455298081544778E-15, -22.50000000000000000 ) ) ;
#8633 = PRODUCT_RELATED_PRODUCT_CATEGORY ( 'part', '', ( #10283 ) ) ;
#8634 = DIRECTION ( 'NONE',  ( 0.000000000000000000, 1.000000000000000000, -0.000000000000000000 ) ) ;
#8635 = AXIS2_PLACEMENT_3D ( 'NONE', #16840, #3799, #1222 ) ;
#8636 = CARTESIAN_POINT ( 'NONE',  ( 0.000000000000000000, 301.0487089519826327, 2.148629195649657075E-12 ) ) ;
#8637 = CARTESIAN_POINT ( 'NONE',  ( -37.00000000000000711, 10.00000000000000000, -18.00000000000000355 ) ) ;
#8638 = DIRECTION ( 'NONE',  ( 0.000000000000000000, 1.000000000000000000, 0.000000000000000000 ) ) ;
#8639 = DIRECTION ( 'NONE',  ( 1.000000000000000000, 0.000000000000000000, 0.000000000000000000 ) ) ;
#8640 = EDGE_LOOP ( 'NONE', ( #15654, #5676, #839, #3983 ) ) ;
#8641 = FACE_OUTER_BOUND ( 'NONE', #3884, .T. ) ;
#8642 = DIRECTION ( 'NONE',  ( 1.000000000000000000, -0.000000000000000000, 0.000000000000000000 ) ) ;
#8643 = EDGE_CURVE ( 'NONE', #4006, #6188, #2205, .T. ) ;
#8644 = CARTESIAN_POINT ( 'NONE',  ( 31.00000000000002842, 68.00000000000000000, 23.00000000000001066 ) ) ;
#8646 = ORIENTED_EDGE ( 'NONE', *, *, #14435, .T. ) ;
#8645 = ORIENTED_EDGE ( 'NONE', *, *, #476, .T. ) ;
#8647 = CARTESIAN_POINT ( 'NONE',  ( 0.9714722756524812874, 38.15493332361022283, 9.451944983354378493 ) ) ;
#8648 = AXIS2_PLACEMENT_3D ( 'NONE', #16555, #15021, #15190 ) ;
#8649 = VERTEX_POINT ( 'NONE', #16308 ) ;
#8650 = CARTESIAN_POINT ( 'NONE',  ( 0.000000000000000000, 10.00000000000000000, 0.000000000000000000 ) ) ;
#8651 = PLANE ( 'NONE',  #8318 ) ;
#8652 = ORIENTED_EDGE ( 'NONE', *, *, #11611, .T. ) ;
#8653 = EDGE_CURVE ( 'NONE', #747, #7006, #9789, .T. ) ;
#8654 = PRODUCT_DEFINITION_CONTEXT ( 'detailed design', #1168, 'design' ) ;
#8655 = DIRECTION ( 'NONE',  ( 0.000000000000000000, 0.000000000000000000, -1.000000000000000000 ) ) ;
#8656 = CARTESIAN_POINT ( 'NONE',  ( 415.3328573526671335, 308.8563596778320743, -6.736600000000000144 ) ) ;
#8657 = EDGE_LOOP ( 'NONE', ( #8619, #15385, #9285, #10267 ) ) ;
#8658 = CARTESIAN_POINT ( 'NONE',  ( -1.512611822017144947, 62.62004896476273785, 9.385845453595075938 ) ) ;
#8659 = AXIS2_PLACEMENT_3D ( 'NONE', #7525, #13037, #15274 ) ;
#8660 = CARTESIAN_POINT ( 'NONE',  ( 0.6999999999999999556, 18.50000000000000000, 0.000000000000000000 ) ) ;
#8661 = CARTESIAN_POINT ( 'NONE',  ( 1.163414460601643398E-15, 38.00000000000000711, 9.500000000000000000 ) ) ;
#8662 = EDGE_CURVE ( 'NONE', #11763, #5640, #3256, .T. ) ;
#8663 = DIRECTION ( 'NONE',  ( 1.000000000000000000, 0.000000000000000000, 0.000000000000000000 ) ) ;
#8664 = CARTESIAN_POINT ( 'NONE',  ( -270.0000000000000000, 620.7506394335853201, -11.00000000000000000 ) ) ;
#8665 = ORIENTED_EDGE ( 'NONE', *, *, #11405, .F. ) ;
#8666 = DIRECTION ( 'NONE',  ( 0.000000000000000000, 0.000000000000000000, 1.000000000000000000 ) ) ;
#8667 = CIRCLE ( 'NONE', #15249, 13.69540538389601991 ) ;
#8668 = DIRECTION ( 'NONE',  ( -1.000000000000000000, -0.000000000000000000, -0.000000000000000000 ) ) ;
#8669 = AXIS2_PLACEMENT_3D ( 'NONE', #1635, #3097, #351 ) ;
#8670 = EDGE_LOOP ( 'NONE', ( #6002, #12978, #6101, #10657 ) ) ;
#8671 = CARTESIAN_POINT ( 'NONE',  ( -31.00000000000000000, 11.00000000000000000, 25.99999999999999645 ) ) ;
#8672 = VERTEX_POINT ( 'NONE', #9951 ) ;
#8673 = EDGE_CURVE ( 'NONE', #6054, #10713, #5972, .T. ) ;
#8674 = PLANE ( 'NONE',  #6923 ) ;
#8675 = DIRECTION ( 'NONE',  ( 0.000000000000000000, 0.000000000000000000, -1.000000000000000000 ) ) ;
#8676 = ORIENTED_EDGE ( 'NONE', *, *, #9078, .F. ) ;
#8677 = CARTESIAN_POINT ( 'NONE',  ( -40.00000000000000711, 10.00000000000000000, 26.00000000000000000 ) ) ;
#8678 = ADVANCED_FACE ( 'NONE', ( #13813 ), #16465, .F. ) ;
#8679 = CARTESIAN_POINT ( 'NONE',  ( 55.99999999999989342, 493.2350855268092573, -589.9613477082210693 ) ) ;
#8680 = DIRECTION ( 'NONE',  ( -0.000000000000000000, -1.000000000000000000, -0.000000000000000000 ) ) ;
#8681 = ORIENTED_EDGE ( 'NONE', *, *, #13395, .T. ) ;
#8682 = EDGE_CURVE ( 'NONE', #15562, #11437, #11652, .T. ) ;
#8683 = AXIS2_PLACEMENT_3D ( 'NONE', #10735, #3190, #16068 ) ;
#8684 = ADVANCED_FACE ( 'NONE', ( #16794 ), #4014, .T. ) ;
#8685 = CIRCLE ( 'NONE', #10877, 13.69540538389598439 ) ;
#8686 = EDGE_CURVE ( 'NONE', #2250, #11869, #13115, .T. ) ;
#8687 = FILL_AREA_STYLE_COLOUR ( '', #8065 ) ;
#8688 = FACE_OUTER_BOUND ( 'NONE', #4977, .T. ) ;
#8689 = ORIENTED_EDGE ( 'NONE', *, *, #6277, .T. ) ;
#8690 = VERTEX_POINT ( 'NONE', #1173 ) ;
#8691 = FACE_OUTER_BOUND ( 'NONE', #1241, .T. ) ;
#8692 = SHAPE_DEFINITION_REPRESENTATION ( #16573, #15822 ) ;
#8693 = DIRECTION ( 'NONE',  ( 0.000000000000000000, 0.000000000000000000, 1.000000000000000000 ) ) ;
#8694 = CARTESIAN_POINT ( 'NONE',  ( 1.831162533324887542, 62.38426314815912832, 9.323294315095143503 ) ) ;
#8695 = VECTOR ( 'NONE', #6560, 1000.000000000000000 ) ;
#8696 = ORIENTED_EDGE ( 'NONE', *, *, #842, .T. ) ;
#8697 = AXIS2_PLACEMENT_3D ( 'NONE', #4938, #7424, #15426 ) ;
#8698 = DIRECTION ( 'NONE',  ( -1.000000000000000000, -0.000000000000000000, -0.000000000000000000 ) ) ;
#8699 = DIRECTION ( 'NONE',  ( -0.000000000000000000, 1.000000000000000000, -0.000000000000000000 ) ) ;
#8700 = ORIENTED_EDGE ( 'NONE', *, *, #7477, .T. ) ;
#8701 = DIRECTION ( 'NONE',  ( -1.000000000000000000, 0.000000000000000000, 1.156482317317881191E-15 ) ) ;
#8702 = LINE ( 'NONE', #13938, #13057 ) ;
#8703 = ORIENTED_EDGE ( 'NONE', *, *, #231, .T. ) ;
#8704 = EDGE_CURVE ( 'NONE', #529, #9900, #14311, .T. ) ;
#8705 = EDGE_CURVE ( 'NONE', #13859, #5920, #16451, .T. ) ;
#8706 = SURFACE_STYLE_USAGE ( .BOTH. , #7056 ) ;
#8707 = ORIENTED_EDGE ( 'NONE', *, *, #14259, .T. ) ;
#8708 = ORIENTED_EDGE ( 'NONE', *, *, #12222, .F. ) ;
#8709 = VECTOR ( 'NONE', #14379, 1000.000000000000000 ) ;
#8710 = AXIS2_PLACEMENT_3D ( 'NONE', #5773, #14721, #5510 ) ;
#8711 = VERTEX_POINT ( 'NONE', #7859 ) ;
#8712 =( NAMED_UNIT ( * ) SI_UNIT ( $, .STERADIAN. ) SOLID_ANGLE_UNIT ( ) );
#8713 = ORIENTED_EDGE ( 'NONE', *, *, #11192, .T. ) ;
#8714 = VERTEX_POINT ( 'NONE', #13033 ) ;
#8715 = DIRECTION ( 'NONE',  ( -0.000000000000000000, -0.000000000000000000, 1.000000000000000000 ) ) ;
#8716 = LINE ( 'NONE', #16431, #13206 ) ;
#8717 = CARTESIAN_POINT ( 'NONE',  ( -31.00000000000001776, 0.000000000000000000, 31.00000000000000000 ) ) ;
#8718 = AXIS2_PLACEMENT_3D ( 'NONE', #2064, #6978, #13921 ) ;
#8719 = DIRECTION ( 'NONE',  ( -0.000000000000000000, -1.000000000000000000, -0.000000000000000000 ) ) ;
#8720 = CARTESIAN_POINT ( 'NONE',  ( 30.99999999999997868, 10.00000000000000000, -30.99999999999999645 ) ) ;
#8721 = DIRECTION ( 'NONE',  ( -1.000000000000000000, -0.000000000000000000, -0.000000000000000000 ) ) ;
#8722 = CARTESIAN_POINT ( 'NONE',  ( 394.0000000000001137, 240.7889724647196488, -110.6822657433598067 ) ) ;
#8723 = CARTESIAN_POINT ( 'NONE',  ( 31.00000000000003553, 10.00000000000000000, -23.00000000000000000 ) ) ;
#8724 = ORIENTED_EDGE ( 'NONE', *, *, #2828, .F. ) ;
#8725 = CARTESIAN_POINT ( 'NONE',  ( 44.99999999999998579, 515.4878487013597805, -546.7230258972048205 ) ) ;
#8726 = CARTESIAN_POINT ( 'NONE',  ( 21.00000000000000000, 19.00000000000000000, -31.00000000000003908 ) ) ;
#8727 = DIRECTION ( 'NONE',  ( 0.000000000000000000, 0.000000000000000000, 1.000000000000000000 ) ) ;
#8729 = VERTEX_POINT ( 'NONE', #16881 ) ;
#8728 = ORIENTED_EDGE ( 'NONE', *, *, #11611, .F. ) ;
#8730 = VECTOR ( 'NONE', #12439, 1000.000000000000000 ) ;
#8731 = CARTESIAN_POINT ( 'NONE',  ( 10.00000000000000000, 372.8685141053783241, -143.5198051533979537 ) ) ;
#8732 = AXIS2_PLACEMENT_3D ( 'NONE', #15883, #6858, #14607 ) ;
#8733 = ORIENTED_EDGE ( 'NONE', *, *, #9100, .T. ) ;
#8734 = CARTESIAN_POINT ( 'NONE',  ( -3.270000000000000462, 285.4366476906530465, 37.52989836422091230 ) ) ;
#8735 = FACE_BOUND ( 'NONE', #2483, .T. ) ;
#8736 = LINE ( 'NONE', #9935, #11883 ) ;
#8737 = ORIENTED_EDGE ( 'NONE', *, *, #16845, .T. ) ;
#8738 = CARTESIAN_POINT ( 'NONE',  ( -270.0000000000000000, 620.7506394335853201, -11.00000000000000000 ) ) ;
#8739 = CARTESIAN_POINT ( 'NONE',  ( -46.99999999999988631, 549.5810598491749488, -575.3306267969850296 ) ) ;
#8740 = ORIENTED_EDGE ( 'NONE', *, *, #3271, .T. ) ;
#8741 = DIRECTION ( 'NONE',  ( 0.000000000000000000, 0.000000000000000000, 1.000000000000000000 ) ) ;
#8742 = VECTOR ( 'NONE', #2217, 1000.000000000000000 ) ;
#8743 = CARTESIAN_POINT ( 'NONE',  ( 0.7365999999999711667, 189.4632308570113537, 37.52989836422062808 ) ) ;
#8744 = DIRECTION ( 'NONE',  ( -0.000000000000000000, -1.000000000000000000, -0.000000000000000000 ) ) ;
#8745 = DIRECTION ( 'NONE',  ( 1.000000000000000000, 0.000000000000000000, 0.000000000000000000 ) ) ;
#8746 = CARTESIAN_POINT ( 'NONE',  ( 31.00000000000001776, 0.000000000000000000, -19.99999999999991473 ) ) ;
#8747 = VERTEX_POINT ( 'NONE', #5031 ) ;
#8748 = LINE ( 'NONE', #932, #708 ) ;
#8749 = EDGE_CURVE ( 'NONE', #9217, #10097, #6229, .T. ) ;
#8750 = DIRECTION ( 'NONE',  ( -1.000000000000000000, 0.000000000000000000, 0.000000000000000000 ) ) ;
#8751 = FACE_OUTER_BOUND ( 'NONE', #10399, .T. ) ;
#8752 = EDGE_CURVE ( 'NONE', #8170, #1977, #2452, .T. ) ;
#8753 = EDGE_CURVE ( 'NONE', #1606, #16501, #15358, .T. ) ;
#8754 = ORIENTED_EDGE ( 'NONE', *, *, #6493, .F. ) ;
#8755 = DIRECTION ( 'NONE',  ( -1.000000000000000000, 0.000000000000000000, 0.000000000000000000 ) ) ;
#8756 = DIRECTION ( 'NONE',  ( 0.000000000000000000, 0.000000000000000000, -1.000000000000000000 ) ) ;
#8757 = ORIENTED_EDGE ( 'NONE', *, *, #16269, .F. ) ;
#8758 = DIRECTION ( 'NONE',  ( 0.000000000000000000, 0.000000000000000000, -1.000000000000000000 ) ) ;
#8759 = CARTESIAN_POINT ( 'NONE',  ( 25.99999999999996092, 3.000000000000000000, -33.99999999999998579 ) ) ;
#8760 = DIRECTION ( 'NONE',  ( 0.000000000000000000, -1.000000000000000000, 0.000000000000000000 ) ) ;
#8761 = ORIENTED_EDGE ( 'NONE', *, *, #3221, .F. ) ;
#8762 = PRODUCT ( '722909', '722909', '', ( #4719 ) ) ;
#8763 = DIRECTION ( 'NONE',  ( -1.000000000000000000, 0.000000000000000000, 0.000000000000000000 ) ) ;
#8764 = CARTESIAN_POINT ( 'NONE',  ( 0.000000000000000000, 0.000000000000000000, 109.9999999999999858 ) ) ;
#8765 = ORIENTED_EDGE ( 'NONE', *, *, #15774, .T. ) ;
#8766 = DIRECTION ( 'NONE',  ( 1.000000000000000000, 0.000000000000000000, -0.000000000000000000 ) ) ;
#8767 = ADVANCED_FACE ( 'NONE', ( #14404 ), #15526, .T. ) ;
#8768 = SHAPE_DEFINITION_REPRESENTATION ( #5051, #2419 ) ;
#8769 = AXIS2_PLACEMENT_3D ( 'NONE', #10065, #5765, #12470 ) ;
#8770 = ADVANCED_FACE ( 'NONE', ( #3764 ), #12935, .F. ) ;
#8771 = CARTESIAN_POINT ( 'NONE',  ( 415.0210210471910841, 329.6061121441327941, -10.00000000000000000 ) ) ;
#8772 = ADVANCED_FACE ( 'NONE', ( #13118 ), #9000, .F. ) ;
#8773 = ORIENTED_EDGE ( 'NONE', *, *, #3913, .F. ) ;
#8774 = EDGE_CURVE ( 'NONE', #11045, #5852, #8919, .T. ) ;
#8775 = CARTESIAN_POINT ( 'NONE',  ( 26.00000000000001066, 0.000000000000000000, -31.00000000000002487 ) ) ;
#8776 = DIRECTION ( 'NONE',  ( 0.000000000000000000, 0.000000000000000000, 1.000000000000000000 ) ) ;
#8777 = ORIENTED_EDGE ( 'NONE', *, *, #5931, .F. ) ;
#8778 = CARTESIAN_POINT ( 'NONE',  ( 449.9999999999998295, 104.2500000000000142, 3.000000000000000000 ) ) ;
#8779 = DIRECTION ( 'NONE',  ( 0.000000000000000000, 0.000000000000000000, 1.000000000000000000 ) ) ;
#8780 = ORIENTED_EDGE ( 'NONE', *, *, #3843, .T. ) ;
#8781 = CIRCLE ( 'NONE', #2738, 13.69540538389601991 ) ;
#8782 = DIRECTION ( 'NONE',  ( -0.000000000000000000, -1.000000000000000000, 0.000000000000000000 ) ) ;
#8783 = VERTEX_POINT ( 'NONE', #5191 ) ;
#8784 = VERTEX_POINT ( 'NONE', #1089 ) ;
#8785 = ORIENTED_EDGE ( 'NONE', *, *, #10182, .F. ) ;
#8786 = ORIENTED_EDGE ( 'NONE', *, *, #506, .F. ) ;
#8787 = EDGE_CURVE ( 'NONE', #12214, #13093, #7942, .T. ) ;
#8788 = EDGE_CURVE ( 'NONE', #3136, #13622, #10445, .T. ) ;
#8789 = VECTOR ( 'NONE', #7716, 1000.000000000000000 ) ;
#8790 = ORIENTED_EDGE ( 'NONE', *, *, #9080, .T. ) ;
#8791 = LINE ( 'NONE', #1205, #5825 ) ;
#8792 = AXIS2_PLACEMENT_3D ( 'NONE', #7074, #12578, #1926 ) ;
#8793 = EDGE_CURVE ( 'NONE', #5039, #6723, #9603, .T. ) ;
#8794 = CARTESIAN_POINT ( 'NONE',  ( 10.00000000000000000, 372.8685141053778693, -83.18019484660869978 ) ) ;
#8795 = DIRECTION ( 'NONE',  ( -1.000000000000000000, 0.000000000000000000, 0.000000000000000000 ) ) ;
#8796 = DIRECTION ( 'NONE',  ( 0.000000000000000000, -0.09950371902098545385, 0.9950371902099903743 ) ) ;
#8797 = CARTESIAN_POINT ( 'NONE',  ( -40.00000000000000000, 19.00000000000000000, 25.99999999999999645 ) ) ;
#8798 = PLANE ( 'NONE',  #1751 ) ;
#8799 = CARTESIAN_POINT ( 'NONE',  ( 0.3969782420128937228, 62.98010902838336023, 9.493666329891928157 ) ) ;
#8800 = FACE_OUTER_BOUND ( 'NONE', #10322, .T. ) ;
#8801 = VERTEX_POINT ( 'NONE', #11818 ) ;
#8802 = CARTESIAN_POINT ( 'NONE',  ( 1.399999999999999911, 0.000000000000000000, 0.000000000000000000 ) ) ;
#8803 = LINE ( 'NONE', #11457, #14605 ) ;
#8804 = AXIS2_PLACEMENT_3D ( 'NONE', #12588, #914, #16699 ) ;
#8805 = SHAPE_REPRESENTATION ( 'din_6885_2_a_6_x_6_x_25', ( #1488 ), #16299 ) ;
#8806 = PLANE ( 'NONE',  #12089 ) ;
#8808 = EDGE_LOOP ( 'NONE', ( #3798, #2350, #2082, #9052 ) ) ;
#8807 = ORIENTED_EDGE ( 'NONE', *, *, #263, .T. ) ;
#8809 = FACE_OUTER_BOUND ( 'NONE', #5297, .T. ) ;
#8810 = VERTEX_POINT ( 'NONE', #61 ) ;
#8811 = CARTESIAN_POINT ( 'NONE',  ( 394.0000000000001137, 341.5974953295075807, -105.4170192159777031 ) ) ;
#8812 = DIRECTION ( 'NONE',  ( 1.000000000000000000, -0.000000000000000000, -0.000000000000000000 ) ) ;
#8813 = AXIS2_PLACEMENT_3D ( 'NONE', #14393, #7669, #10280 ) ;
#8814 = ORIENTED_EDGE ( 'NONE', *, *, #14119, .F. ) ;
#8815 = UNCERTAINTY_MEASURE_WITH_UNIT (LENGTH_MEASURE( 1.000000000000000082E-05 ), #13272, 'distance_accuracy_value', 'NONE');
#8816 = LINE ( 'NONE', #3413, #14946 ) ;
#8817 = CARTESIAN_POINT ( 'NONE',  ( 31.00000000000006395, 68.00000000000000000, -22.99999999999999289 ) ) ;
#8818 = EDGE_LOOP ( 'NONE', ( #13886, #4559, #5606, #3720 ) ) ;
#8819 = CARTESIAN_POINT ( 'NONE',  ( 35.99999999999999289, 8.000000000000000000, 21.99999999999999645 ) ) ;
#8820 = FACE_BOUND ( 'NONE', #2751, .T. ) ;
#8821 = LINE ( 'NONE', #844, #15960 ) ;
#8822 = CARTESIAN_POINT ( 'NONE',  ( 35.99999999999999289, 8.000000000000000000, 21.99999999999999645 ) ) ;
#8823 = DIRECTION ( 'NONE',  ( -0.000000000000000000, -1.000000000000000000, -0.000000000000000000 ) ) ;
#8824 = ADVANCED_FACE ( 'NONE', ( #7605, #15769 ), #6650, .T. ) ;
#8825 = ORIENTED_EDGE ( 'NONE', *, *, #14116, .F. ) ;
#8826 = VECTOR ( 'NONE', #7048, 1000.000000000000000 ) ;
#8827 = CARTESIAN_POINT ( 'NONE',  ( 32.99999999999998579, 8.000000000000000000, 25.99999999999999645 ) ) ;
#8828 = VECTOR ( 'NONE', #15871, 1000.000000000000000 ) ;
#8829 = EDGE_CURVE ( 'NONE', #5615, #8853, #16196, .T. ) ;
#8830 = CARTESIAN_POINT ( 'NONE',  ( 37.00000000000003553, 3.000000000000000000, 20.00000000000000000 ) ) ;
#8831 = CLOSED_SHELL ( 'NONE', ( #7201, #11186, #16749, #3757, #12338, #4740, #5742, #7883, #7277, #14496, #12189, #16311 ) ) ;
#8832 = CARTESIAN_POINT ( 'NONE',  ( 39.99999999999999289, 10.00000000000000000, -26.00000000000000000 ) ) ;
#8833 = ORIENTED_EDGE ( 'NONE', *, *, #10576, .T. ) ;
#8834 = PLANE ( 'NONE',  #3091 ) ;
#8835 = VECTOR ( 'NONE', #12026, 1000.000000000000000 ) ;
#8836 = PRODUCT_RELATED_PRODUCT_CATEGORY ( 'part', '', ( #2443 ) ) ;
#8837 = DIRECTION ( 'NONE',  ( 0.000000000000000000, 0.000000000000000000, 1.000000000000000000 ) ) ;
#8838 = ORIENTED_EDGE ( 'NONE', *, *, #13509, .F. ) ;
#8839 = CARTESIAN_POINT ( 'NONE',  ( -22.99999999999999645, 68.00000000000000000, 37.00000000000002132 ) ) ;
#8840 = DIRECTION ( 'NONE',  ( 0.000000000000000000, -1.000000000000000000, 0.000000000000000000 ) ) ;
#8841 = DIRECTION ( 'NONE',  ( 3.491481338843132566E-15, 0.9950371902099890420, -0.09950371902099952592 ) ) ;
#8842 = ORIENTED_EDGE ( 'NONE', *, *, #5836, .T. ) ;
#8843 = CARTESIAN_POINT ( 'NONE',  ( 35.99999999999999289, 10.00000000000000000, 21.99999999999999645 ) ) ;
#8844 = AXIS2_PLACEMENT_3D ( 'NONE', #13139, #9276, #7803 ) ;
#8845 = DIRECTION ( 'NONE',  ( -1.000000000000000000, -0.000000000000000000, -0.000000000000000000 ) ) ;
#8846 = DIRECTION ( 'NONE',  ( 0.000000000000000000, 1.000000000000000000, 0.000000000000000000 ) ) ;
#8847 = EDGE_LOOP ( 'NONE', ( #2618, #5947, #1243, #5508 ) ) ;
#8848 = EDGE_CURVE ( 'NONE', #6167, #2142, #153, .T. ) ;
#8849 = LINE ( 'NONE', #2315, #7801 ) ;
#8850 = APPLICATION_CONTEXT ( 'automotive_design' ) ;
#8851 = CIRCLE ( 'NONE', #15981, 9.000000000000007105 ) ;
#8852 = CARTESIAN_POINT ( 'NONE',  ( -33.00000000000000000, 8.000000000000000000, -22.00000000000000355 ) ) ;
#8853 = VERTEX_POINT ( 'NONE', #16115 ) ;
#8854 = MECHANICAL_DESIGN_GEOMETRIC_PRESENTATION_REPRESENTATION (  '', ( #4201 ), #16263 ) ;
#8855 = CARTESIAN_POINT ( 'NONE',  ( 0.000000000000000000, 306.0487089519837696, -155.0000000000038369 ) ) ;
#8856 = FACE_OUTER_BOUND ( 'NONE', #12102, .T. ) ;
#8857 = EDGE_CURVE ( 'NONE', #8258, #1983, #558, .T. ) ;
#8858 = DIRECTION ( 'NONE',  ( -0.000000000000000000, -1.000000000000000000, -0.000000000000000000 ) ) ;
#8859 = ORIENTED_EDGE ( 'NONE', *, *, #1765, .F. ) ;
#8860 = CARTESIAN_POINT ( 'NONE',  ( 394.0000000000001137, 240.7889724647196488, -104.2090657433598011 ) ) ;
#8861 = CARTESIAN_POINT ( 'NONE',  ( -45.00000000000000000, 473.6663340069157471, -531.5012393965008641 ) ) ;
#8862 = EDGE_LOOP ( 'NONE', ( #12815, #9734, #6129, #12586 ) ) ;
#8863 = CIRCLE ( 'NONE', #12428, 8.000000000000000000 ) ;
#8864 = DIRECTION ( 'NONE',  ( 1.000000000000000000, 1.597771622610217359E-16, 0.000000000000000000 ) ) ;
#8865 = ORIENTED_EDGE ( 'NONE', *, *, #9670, .F. ) ;
#8866 = ADVANCED_FACE ( 'NONE', ( #2976 ), #4929, .T. ) ;
#8867 = ORIENTED_EDGE ( 'NONE', *, *, #3092, .T. ) ;
#8868 = MECHANICAL_DESIGN_GEOMETRIC_PRESENTATION_REPRESENTATION (  '', ( #14342 ), #12718 ) ;
#8869 = EDGE_CURVE ( 'NONE', #6506, #13502, #6848, .T. ) ;
#8870 = CARTESIAN_POINT ( 'NONE',  ( 31.00000000000000711, 68.00000000000000000, -30.99999999999999289 ) ) ;
#8871 = VECTOR ( 'NONE', #3329, 1000.000000000000000 ) ;
#8872 = AXIS2_PLACEMENT_3D ( 'NONE', #12800, #15370, #8846 ) ;
#8873 = CIRCLE ( 'NONE', #1462, 3.300000000000011369 ) ;
#8874 = ORIENTED_EDGE ( 'NONE', *, *, #5499, .F. ) ;
#8875 = ORIENTED_EDGE ( 'NONE', *, *, #9929, .F. ) ;
#8876 = VECTOR ( 'NONE', #13417, 1000.000000000000000 ) ;
#8877 = ORIENTED_EDGE ( 'NONE', *, *, #12768, .F. ) ;
#8878 = DIRECTION ( 'NONE',  ( -1.000000000000000000, 0.000000000000000000, 0.000000000000000000 ) ) ;
#8879 = LINE ( 'NONE', #14369, #5300 ) ;
#8880 = MECHANICAL_DESIGN_GEOMETRIC_PRESENTATION_REPRESENTATION (  '', ( #9433 ), #15725 ) ;
#8881 = VECTOR ( 'NONE', #10363, 1000.000000000000114 ) ;
#8882 = EDGE_CURVE ( 'NONE', #13599, #12411, #13449, .T. ) ;
#8883 = DIRECTION ( 'NONE',  ( 1.000000000000000000, -0.000000000000000000, 0.000000000000000000 ) ) ;
#8884 = PLANE ( 'NONE',  #6371 ) ;
#8885 = VECTOR ( 'NONE', #5624, 1000.000000000000000 ) ;
#8886 = DIRECTION ( 'NONE',  ( 0.000000000000000000, 1.000000000000000000, 0.000000000000000000 ) ) ;
#8887 = LINE ( 'NONE', #8970, #8521 ) ;
#8888 = CYLINDRICAL_SURFACE ( 'NONE', #9135, 8.000000000000000000 ) ;
#8889 = EDGE_CURVE ( 'NONE', #16672, #8784, #5455, .T. ) ;
#8890 = ORIENTED_EDGE ( 'NONE', *, *, #5, .F. ) ;
#8891 = LINE ( 'NONE', #3565, #1569 ) ;
#8892 = DIRECTION ( 'NONE',  ( 0.000000000000000000, 0.000000000000000000, 1.000000000000000000 ) ) ;
#8893 = CIRCLE ( 'NONE', #401, 4.695405383896011919 ) ;
#8894 = ORIENTED_EDGE ( 'NONE', *, *, #3573, .T. ) ;
#8895 = EDGE_CURVE ( 'NONE', #2103, #16003, #14668, .T. ) ;
#8896 = EDGE_CURVE ( 'NONE', #7385, #3015, #8129, .T. ) ;
#8897 = EDGE_CURVE ( 'NONE', #1411, #1755, #9331, .T. ) ;
#8898 = CARTESIAN_POINT ( 'NONE',  ( -31.00000000000003197, 68.00000000000000000, 26.00000000000000355 ) ) ;
#8900 = ORIENTED_EDGE ( 'NONE', *, *, #9740, .F. ) ;
#8899 = ORIENTED_EDGE ( 'NONE', *, *, #9882, .F. ) ;
#8901 = AXIS2_PLACEMENT_3D ( 'NONE', #6954, #3357, #11330 ) ;
#8902 = FACE_OUTER_BOUND ( 'NONE', #4331, .T. ) ;
#8903 = VECTOR ( 'NONE', #543, 1000.000000000000000 ) ;
#8904 = FACE_BOUND ( 'NONE', #10082, .T. ) ;
#8905 = VECTOR ( 'NONE', #9215, 1000.000000000000000 ) ;
#8906 = PLANE ( 'NONE',  #3593 ) ;
#8907 = DIRECTION ( 'NONE',  ( 1.000000000000000000, 0.000000000000000000, -0.000000000000000000 ) ) ;
#8908 = EDGE_LOOP ( 'NONE', ( #13929, #121, #1507, #5589 ) ) ;
#8909 = CYLINDRICAL_SURFACE ( 'NONE', #16550, 3.300000000000000711 ) ;
#8910 = PRODUCT_DEFINITION_FORMATION_WITH_SPECIFIED_SOURCE ( 'ANY', '', #3694, .NOT_KNOWN. ) ;
#8911 = EDGE_LOOP ( 'NONE', ( #2066, #16832, #5073, #1399 ) ) ;
#8912 = LINE ( 'NONE', #14150, #2201 ) ;
#8913 = AXIS2_PLACEMENT_3D ( 'NONE', #16788, #5269, #52 ) ;
#8914 = CARTESIAN_POINT ( 'NONE',  ( 0.6444877810228004655, 192.7531883598551872, 37.23446286945478079 ) ) ;
#8915 = CARTESIAN_POINT ( 'NONE',  ( 55.99999999999989342, 493.2350855268092573, -585.2659423243250103 ) ) ;
#8916 = AXIS2_PLACEMENT_3D ( 'NONE', #2917, #10818, #13406 ) ;
#8917 = EDGE_CURVE ( 'NONE', #5045, #8217, #9684, .T. ) ;
#8918 = DIRECTION ( 'NONE',  ( 1.000000000000000000, 0.000000000000000000, 0.000000000000000000 ) ) ;
#8919 = LINE ( 'NONE', #10197, #1645 ) ;
#8920 = ORIENTED_EDGE ( 'NONE', *, *, #4886, .F. ) ;
#8921 = CARTESIAN_POINT ( 'NONE',  ( -37.00000000000000711, 0.000000000000000000, -23.00000000000000000 ) ) ;
#8922 = LINE ( 'NONE', #11743, #2237 ) ;
#8923 = CARTESIAN_POINT ( 'NONE',  ( 20.99999999999996092, -20.00000000000000000, 37.50000000000001421 ) ) ;
#8924 = VERTEX_POINT ( 'NONE', #12082 ) ;
#8925 = AXIS2_PLACEMENT_3D ( 'NONE', #415, #10448, #15772 ) ;
#8926 = DIRECTION ( 'NONE',  ( 6.123031769111888756E-17, -1.000000000000000000, -3.749151804555344967E-33 ) ) ;
#8927 = EDGE_CURVE ( 'NONE', #4210, #16153, #6911, .T. ) ;
#8928 = CARTESIAN_POINT ( 'NONE',  ( -19.00000000000001776, 8.000000000000000000, 40.00000000000000711 ) ) ;
#8929 = VERTEX_POINT ( 'NONE', #5638 ) ;
#8930 = FACE_OUTER_BOUND ( 'NONE', #10485, .T. ) ;
#8931 = CARTESIAN_POINT ( 'NONE',  ( -21.00000000000002842, 3.000000000000000000, -34.99999999999999289 ) ) ;
#8932 = FACE_BOUND ( 'NONE', #1668, .T. ) ;
#8933 = ORIENTED_EDGE ( 'NONE', *, *, #9489, .T. ) ;
#8934 = CARTESIAN_POINT ( 'NONE',  ( -26.00000000000002132, 0.000000000000000000, -31.00000000000003553 ) ) ;
#8935 = DIRECTION ( 'NONE',  ( -0.000000000000000000, 1.000000000000000000, -0.000000000000000000 ) ) ;
#8936 = ORIENTED_EDGE ( 'NONE', *, *, #589, .T. ) ;
#8937 = FACE_OUTER_BOUND ( 'NONE', #657, .T. ) ;
#8938 = VECTOR ( 'NONE', #4310, 1000.000000000000000 ) ;
#8939 = MANIFOLD_SOLID_BREP ( 'Cut-Extrude1[1]', #8548 ) ;
#8940 = ORIENTED_EDGE ( 'NONE', *, *, #15396, .T. ) ;
#8941 = FACE_OUTER_BOUND ( 'NONE', #9908, .T. ) ;
#8942 = CARTESIAN_POINT ( 'NONE',  ( 415.3328573526671335, 308.8563596778320743, 0.000000000000000000 ) ) ;
#8943 = AXIS2_PLACEMENT_3D ( 'NONE', #12954, #5133, #10384 ) ;
#8944 = DIRECTION ( 'NONE',  ( 0.000000000000000000, 1.000000000000000000, 0.000000000000000000 ) ) ;
#8945 = EDGE_LOOP ( 'NONE', ( #14047, #15164, #5220, #5337, #15517 ) ) ;
#8946 = AXIS2_PLACEMENT_3D ( 'NONE', #15782, #13392, #14503 ) ;
#8947 = DIRECTION ( 'NONE',  ( 0.000000000000000000, 0.000000000000000000, 1.000000000000000000 ) ) ;
#8948 = FACE_OUTER_BOUND ( 'NONE', #1729, .T. ) ;
#8949 = ORIENTED_EDGE ( 'NONE', *, *, #1734, .T. ) ;
#8950 = CARTESIAN_POINT ( 'NONE',  ( 31.81980515339464333, 0.000000000000000000, -31.81980515339463622 ) ) ;
#8951 = ORIENTED_EDGE ( 'NONE', *, *, #12341, .F. ) ;
#8952 = EDGE_LOOP ( 'NONE', ( #2166, #302, #16484, #2115 ) ) ;
#8953 = FACE_OUTER_BOUND ( 'NONE', #4526, .T. ) ;
#8954 = ORIENTED_EDGE ( 'NONE', *, *, #6023, .F. ) ;
#8955 = DIRECTION ( 'NONE',  ( 1.000000000000000000, 0.000000000000000000, 0.000000000000000000 ) ) ;
#8956 = PRODUCT_DEFINITION_CONTEXT ( 'detailed design', #2371, 'design' ) ;
#8957 = VECTOR ( 'NONE', #13479, 1000.000000000000000 ) ;
#8958 = EDGE_CURVE ( 'NONE', #16701, #15, #9591, .T. ) ;
#8959 = AXIS2_PLACEMENT_3D ( 'NONE', #1906, #12388, #8445 ) ;
#8960 = ORIENTED_EDGE ( 'NONE', *, *, #7781, .F. ) ;
#8961 = ORIENTED_EDGE ( 'NONE', *, *, #7184, .T. ) ;
#8962 = CARTESIAN_POINT ( 'NONE',  ( 0.000000000000000000, 240.0523724647196389, -104.2090657433598011 ) ) ;
#8963 = CARTESIAN_POINT ( 'NONE',  ( -25.99999999999999645, 68.00000000000000000, -39.99999999999999289 ) ) ;
#8964 = EDGE_CURVE ( 'NONE', #8520, #15272, #11044, .T. ) ;
#8965 = EDGE_CURVE ( 'NONE', #9650, #11502, #11378, .T. ) ;
#8966 = ORIENTED_EDGE ( 'NONE', *, *, #5841, .T. ) ;
#8967 = CARTESIAN_POINT ( 'NONE',  ( -39.99999999999997868, 0.000000000000000000, 26.00000000000000355 ) ) ;
#8968 = LINE ( 'NONE', #2507, #16561 ) ;
#8969 = VECTOR ( 'NONE', #3234, 1000.000000000000000 ) ;
#8970 = CARTESIAN_POINT ( 'NONE',  ( 19.99999999999995381, 3.000000000000000000, -36.99999999999999289 ) ) ;
#8971 = AXIS2_PLACEMENT_3D ( 'NONE', #14188, #14352, #10321 ) ;
#8972 = CARTESIAN_POINT ( 'NONE',  ( -55.99999999999989342, 493.2350855268092573, -585.2659423243250103 ) ) ;
#8973 = VERTEX_POINT ( 'NONE', #13638 ) ;
#8974 = CARTESIAN_POINT ( 'NONE',  ( -33.99999999999997158, 3.000000000000000000, -25.99999999999999645 ) ) ;
#8975 = CARTESIAN_POINT ( 'NONE',  ( 394.0000000000001137, 240.7889724647196488, -10.68226574335980139 ) ) ;
#8976 = ORIENTED_EDGE ( 'NONE', *, *, #15481, .T. ) ;
#8977 = FACE_OUTER_BOUND ( 'NONE', #11169, .T. ) ;
#8978 = ORIENTED_EDGE ( 'NONE', *, *, #16537, .F. ) ;
#8979 =( REPRESENTATION_RELATIONSHIP ('NONE','NONE', #15277, #15920 ) REPRESENTATION_RELATIONSHIP_WITH_TRANSFORMATION ( #12717 )SHAPE_REPRESENTATION_RELATIONSHIP( ) );
#8980 = FACE_OUTER_BOUND ( 'NONE', #7158, .T. ) ;
#8981 = ADVANCED_FACE ( 'NONE', ( #7333 ), #12669, .F. ) ;
#8982 = ORIENTED_EDGE ( 'NONE', *, *, #14435, .F. ) ;
#8983 = AXIS2_PLACEMENT_3D ( 'NONE', #10386, #10306, #3780 ) ;
#8984 = ORIENTED_EDGE ( 'NONE', *, *, #7392, .T. ) ;
#8985 = DIRECTION ( 'NONE',  ( 0.000000000000000000, 0.000000000000000000, 1.000000000000000000 ) ) ;
#8986 = DIRECTION ( 'NONE',  ( 0.000000000000000000, -1.000000000000000000, 0.000000000000000000 ) ) ;
#8987 = ADVANCED_FACE ( 'NONE', ( #7248 ), #16616, .F. ) ;
#8988 = DIRECTION ( 'NONE',  ( 0.000000000000000000, -1.000000000000000000, -1.321694076934710402E-16 ) ) ;
#8989 = EDGE_CURVE ( 'NONE', #9577, #197, #2017, .T. ) ;
#8991 = ORIENTED_EDGE ( 'NONE', *, *, #12740, .F. ) ;
#8990 = ADVANCED_FACE ( 'NONE', ( #15003 ), #6046, .F. ) ;
#8992 = EDGE_CURVE ( 'NONE', #14337, #276, #4114, .T. ) ;
#8993 = DIRECTION ( 'NONE',  ( 0.000000000000000000, 0.000000000000000000, 1.000000000000000000 ) ) ;
#8994 = ORIENTED_EDGE ( 'NONE', *, *, #6969, .F. ) ;
#8995 = CARTESIAN_POINT ( 'NONE',  ( -37.00000000000000711, 10.00000000000000000, 23.00000000000000000 ) ) ;
#8996 = CARTESIAN_POINT ( 'NONE',  ( 1.231993379943791155E-12, 193.4898140233672450, 37.52989836422092651 ) ) ;
#8997 = DIRECTION ( 'NONE',  ( -0.000000000000000000, 1.000000000000000000, -0.000000000000000000 ) ) ;
#8998 = PRESENTATION_LAYER_ASSIGNMENT (  '', '', ( #222 ) ) ;
#8999 = CARTESIAN_POINT ( 'NONE',  ( 55.99999999999989342, 523.2161522479893847, -590.5524132976893270 ) ) ;
#9000 = PLANE ( 'NONE',  #13986 ) ;
#9002 = EDGE_LOOP ( 'NONE', ( #2433, #3652, #10356, #14510 ) ) ;
#9001 = ORIENTED_EDGE ( 'NONE', *, *, #6174, .F. ) ;
#9003 = DIRECTION ( 'NONE',  ( 0.000000000000000000, 0.000000000000000000, 1.000000000000000000 ) ) ;
#9004 = CARTESIAN_POINT ( 'NONE',  ( 0.000000000000000000, 226.8713558223388134, -358.7582248962859808 ) ) ;
#9005 = ADVANCED_FACE ( 'NONE', ( #15076 ), #5888, .F. ) ;
#9006 = CARTESIAN_POINT ( 'NONE',  ( 30.99999999999999645, 0.000000000000000000, 31.00000000000001066 ) ) ;
#9007 = VERTEX_POINT ( 'NONE', #746 ) ;
#9008 = EDGE_CURVE ( 'NONE', #2065, #1379, #11289, .T. ) ;
#9009 = VECTOR ( 'NONE', #6596, 1000.000000000000000 ) ;
#9010 = CARTESIAN_POINT ( 'NONE',  ( -40.00000000000000000, 0.000000000000000000, 26.00000000000000355 ) ) ;
#9011 = FACE_OUTER_BOUND ( 'NONE', #10915, .T. ) ;
#9012 = VERTEX_POINT ( 'NONE', #16447 ) ;
#9013 = CARTESIAN_POINT ( 'NONE',  ( 46.99999999999988631, 473.6663340069157471, -536.1966447803968094 ) ) ;
#9014 = FACE_OUTER_BOUND ( 'NONE', #14619, .T. ) ;
#9015 = CARTESIAN_POINT ( 'NONE',  ( 36.99999999999999289, 10.00000000000000000, 22.99999999999999645 ) ) ;
#9016 = ORIENTED_EDGE ( 'NONE', *, *, #281, .F. ) ;
#9017 = CARTESIAN_POINT ( 'NONE',  ( 0.7365999999999783832, 260.4765148507123058, 287.1312267635910871 ) ) ;
#9018 = CARTESIAN_POINT ( 'NONE',  ( 10.00000000000000000, 5.352861011586007481E-13, -75.00000000000599698 ) ) ;
#9019 = LINE ( 'NONE', #6583, #341 ) ;
#9020 = ORIENTED_EDGE ( 'NONE', *, *, #12053, .T. ) ;
#9021 = DIRECTION ( 'NONE',  ( 0.000000000000000000, 0.000000000000000000, 1.000000000000000000 ) ) ;
#9022 = CIRCLE ( 'NONE', #4894, 13.69540538389598794 ) ;
#9023 = EDGE_CURVE ( 'NONE', #11441, #15661, #4672, .T. ) ;
#9024 = CONTEXT_DEPENDENT_SHAPE_REPRESENTATION ( #16099, #6840 ) ;
#9025 = ORIENTED_EDGE ( 'NONE', *, *, #12830, .F. ) ;
#9026 = FACE_OUTER_BOUND ( 'NONE', #1040, .T. ) ;
#9027 = CARTESIAN_POINT ( 'NONE',  ( 394.0000000000001137, 339.3157724647196005, -16.41886574335978821 ) ) ;
#9028 = FACE_OUTER_BOUND ( 'NONE', #706, .T. ) ;
#9029 = ORIENTED_EDGE ( 'NONE', *, *, #12568, .F. ) ;
#9030 = DIRECTION ( 'NONE',  ( -0.000000000000000000, -0.000000000000000000, 1.000000000000000000 ) ) ;
#9031 = AXIS2_PLACEMENT_3D ( 'NONE', #12751, #8639, #649 ) ;
#9032 = DIRECTION ( 'NONE',  ( 0.000000000000000000, 0.000000000000000000, 1.000000000000000000 ) ) ;
#9033 = EDGE_LOOP ( 'NONE', ( #395, #1090 ) ) ;
#9034 = CARTESIAN_POINT ( 'NONE',  ( -32.00000000000000711, 10.00000000000000000, -22.00000000000000355 ) ) ;
#9035 = ORIENTED_EDGE ( 'NONE', *, *, #9811, .T. ) ;
#9036 = EDGE_LOOP ( 'NONE', ( #7547, #7534, #15937, #9999 ) ) ;
#9037 = AXIS2_PLACEMENT_3D ( 'NONE', #12606, #2297, #3844 ) ;
#9038 = DIRECTION ( 'NONE',  ( -0.000000000000000000, -1.000000000000000000, -0.000000000000000000 ) ) ;
#9039 = EDGE_LOOP ( 'NONE', ( #4161, #13096, #13012, #14272, #881, #7667 ) ) ;
#9040 = PRODUCT ( 'HG-KN73JK', 'HG-KN73JK', '', ( #14963 ) ) ;
#9041 = EDGE_LOOP ( 'NONE', ( #16922, #15392, #12673, #1371 ) ) ;
#9042 = ORIENTED_EDGE ( 'NONE', *, *, #2966, .T. ) ;
#9043 = CARTESIAN_POINT ( 'NONE',  ( 40.00000000000000711, 8.000000000000000000, -34.99999999999997868 ) ) ;
#9044 = EDGE_LOOP ( 'NONE', ( #8994, #14736, #187, #8681 ) ) ;
#9045 = CARTESIAN_POINT ( 'NONE',  ( 3.324999999999999734, 0.000000000000000000, 0.000000000000000000 ) ) ;
#9046 =( NAMED_UNIT ( * ) SI_UNIT ( $, .STERADIAN. ) SOLID_ANGLE_UNIT ( ) );
#9047 = ADVANCED_FACE ( 'NONE', ( #8473, #10095 ), #15159, .F. ) ;
#9048 = CARTESIAN_POINT ( 'NONE',  ( -31.00000000000000000, 19.00000000000000000, -31.00000000000000000 ) ) ;
#9049 = ORIENTED_EDGE ( 'NONE', *, *, #13377, .T. ) ;
#9050 = CARTESIAN_POINT ( 'NONE',  ( 35.00000000000003553, 0.000000000000000000, -18.49999999999999645 ) ) ;
#9051 = FACE_OUTER_BOUND ( 'NONE', #4420, .T. ) ;
#9052 = ORIENTED_EDGE ( 'NONE', *, *, #4280, .T. ) ;
#9053 = DIRECTION ( 'NONE',  ( 1.000000000000000000, -0.000000000000000000, 0.000000000000000000 ) ) ;
#9054 = ORIENTED_EDGE ( 'NONE', *, *, #11715, .T. ) ;
#9055 = EDGE_CURVE ( 'NONE', #9546, #8177, #4759, .T. ) ;
#9056 = AXIS2_PLACEMENT_3D ( 'NONE', #10424, #9145, #3567 ) ;
#9057 = AXIS2_PLACEMENT_3D ( 'NONE', #10128, #10382, #3853 ) ;
#9058 = EDGE_LOOP ( 'NONE', ( #6392, #160, #4648, #10997 ) ) ;
#9059 = VERTEX_POINT ( 'NONE', #13710 ) ;
#9060 = CARTESIAN_POINT ( 'NONE',  ( 34.00000000000002842, -20.00000000000000000, 26.00000000000000355 ) ) ;
#9061 = COLOUR_RGB ( '', 0.09019608, 0.27058824, 0.51372549) ;
#9062 = DIRECTION ( 'NONE',  ( -3.407805566942604749E-15, -0.9950371902099890420, 0.09950371902099952592 ) ) ;
#9063 = CARTESIAN_POINT ( 'NONE',  ( 55.99999999999989342, 549.5810598491746077, -504.4200196135282113 ) ) ;
#9064 = VERTEX_POINT ( 'NONE', #1935 ) ;
#9065 = CARTESIAN_POINT ( 'NONE',  ( -150.0000000000000000, 512.1906115401388888, -11.00000000000000000 ) ) ;
#9066 = PLANE ( 'NONE',  #8913 ) ;
#9067 = AXIS2_PLACEMENT_3D ( 'NONE', #11980, #218, #10682 ) ;
#9068 = EDGE_CURVE ( 'NONE', #4162, #4234, #7079, .T. ) ;
#9069 = FACE_OUTER_BOUND ( 'NONE', #432, .T. ) ;
#9070 = ADVANCED_FACE ( 'NONE', ( #4600 ), #15251, .T. ) ;
#9071 = FACE_BOUND ( 'NONE', #15949, .T. ) ;
#9072 = DIRECTION ( 'NONE',  ( -1.000000000000000000, -0.000000000000000000, 0.000000000000000000 ) ) ;
#9073 = CARTESIAN_POINT ( 'NONE',  ( -25.99999999999999645, 68.00000000000000000, 40.00000000000002132 ) ) ;
#9074 = CARTESIAN_POINT ( 'NONE',  ( 0.7366000000000204606, 214.4632308570090800, 287.5298983642209123 ) ) ;
#9076 = ORIENTED_EDGE ( 'NONE', *, *, #2476, .T. ) ;
#9075 = EDGE_LOOP ( 'NONE', ( #2872, #9237, #15660, #13157 ) ) ;
#9077 = EDGE_CURVE ( 'NONE', #3627, #15036, #3022, .T. ) ;
#9078 = EDGE_CURVE ( 'NONE', #12512, #4334, #7584, .T. ) ;
#9079 = CARTESIAN_POINT ( 'NONE',  ( -40.00000000000000000, 68.00000000000000000, 26.00000000000000355 ) ) ;
#9080 = EDGE_CURVE ( 'NONE', #4316, #11045, #14278, .T. ) ;
#9081 = AXIS2_PLACEMENT_3D ( 'NONE', #8650, #15172, #833 ) ;
#9082 = DIRECTION ( 'NONE',  ( 1.000000000000000000, 0.000000000000000000, 0.000000000000000000 ) ) ;
#9083 = DIRECTION ( 'NONE',  ( -1.000000000000000000, 0.000000000000000000, 0.000000000000000000 ) ) ;
#9084 = ORIENTED_EDGE ( 'NONE', *, *, #7206, .T. ) ;
#9085 = DIRECTION ( 'NONE',  ( 1.000000000000000000, 0.000000000000000000, -0.000000000000000000 ) ) ;
#9086 = LINE ( 'NONE', #12950, #7841 ) ;
#9088 = EDGE_CURVE ( 'NONE', #16656, #14275, #16863, .T. ) ;
#9087 = VERTEX_POINT ( 'NONE', #16775 ) ;
#9089 = FACE_OUTER_BOUND ( 'NONE', #4182, .T. ) ;
#9090 = CARTESIAN_POINT ( 'NONE',  ( 26.00000000000000000, 19.00000000000000000, -40.00000000000000711 ) ) ;
#9091 = DIRECTION ( 'NONE',  ( 1.000000000000000000, 0.000000000000000000, -0.000000000000000000 ) ) ;
#9092 = VERTEX_POINT ( 'NONE', #11630 ) ;
#9093 = CIRCLE ( 'NONE', #14299, 22.75209553982837463 ) ;
#9094 = CARTESIAN_POINT ( 'NONE',  ( 35.00000000000000711, 19.00000000000000000, 20.99999999999999289 ) ) ;
#9095 = CARTESIAN_POINT ( 'NONE',  ( -430.0000000000000568, 620.7506394335853201, 109.9999999999999858 ) ) ;
#9096 = DIRECTION ( 'NONE',  ( 0.000000000000000000, 0.000000000000000000, -1.000000000000000000 ) ) ;
#9097 = ORIENTED_EDGE ( 'NONE', *, *, #14654, .F. ) ;
#9098 = EDGE_CURVE ( 'NONE', #9930, #14326, #1242, .T. ) ;
#9099 = EDGE_CURVE ( 'NONE', #1899, #9971, #2432, .T. ) ;
#9100 = EDGE_CURVE ( 'NONE', #4422, #4924, #12756, .T. ) ;
#9101 = CYLINDRICAL_SURFACE ( 'NONE', #2038, 3.299999999999997158 ) ;
#9102 = EDGE_CURVE ( 'NONE', #4981, #15644, #3902, .T. ) ;
#9103 = CLOSED_SHELL ( 'NONE', ( #8378, #1957, #8440, #9200, #16821, #9070, #9133, #2456, #12098, #14185, #7798, #5717, #14458, #14179, #13423 ) ) ;
#9104 = VECTOR ( 'NONE', #16799, 1000.000000000000000 ) ;
#9105 = CARTESIAN_POINT ( 'NONE',  ( 56.73000000000001108, 192.7170024689953891, 37.20452120302224586 ) ) ;
#9106 = AXIS2_PLACEMENT_3D ( 'NONE', #16678, #640, #7322 ) ;
#9107 = ORIENTED_EDGE ( 'NONE', *, *, #13398, .F. ) ;
#9108 = DIRECTION ( 'NONE',  ( -1.000000000000000000, 0.000000000000000000, -5.782411586589400040E-16 ) ) ;
#9109 = DIRECTION ( 'NONE',  ( 0.000000000000000000, 1.000000000000000000, 0.000000000000000000 ) ) ;
#9110 = VECTOR ( 'NONE', #1252, 1000.000000000000000 ) ;
#9111 = CARTESIAN_POINT ( 'NONE',  ( 45.00000000000000000, 549.5810598491746077, -504.4200196135282113 ) ) ;
#9112 = ORIENTED_EDGE ( 'NONE', *, *, #7754, .F. ) ;
#9113 = FACE_OUTER_BOUND ( 'NONE', #4448, .T. ) ;
#9114 = AXIS2_PLACEMENT_3D ( 'NONE', #15662, #7591, #8198 ) ;
#9115 = CARTESIAN_POINT ( 'NONE',  ( -23.00000000000002132, 0.000000000000000000, 37.00000000000000711 ) ) ;
#9116 = VERTEX_POINT ( 'NONE', #7661 ) ;
#9117 = PLANE ( 'NONE',  #13553 ) ;
#9118 = ORIENTED_EDGE ( 'NONE', *, *, #4973, .T. ) ;
#9119 = EDGE_LOOP ( 'NONE', ( #15072, #3380, #15486, #8192 ) ) ;
#9120 = AXIS2_PLACEMENT_3D ( 'NONE', #10144, #3787, #3616 ) ;
#9121 = DIRECTION ( 'NONE',  ( -1.000000000000000000, 0.000000000000000000, -0.000000000000000000 ) ) ;
#9122 = VERTEX_POINT ( 'NONE', #11795 ) ;
#9123 =( NAMED_UNIT ( * ) PLANE_ANGLE_UNIT ( ) SI_UNIT ( $, .RADIAN. ) );
#9124 = VECTOR ( 'NONE', #234, 1000.000000000000000 ) ;
#9125 = ORIENTED_EDGE ( 'NONE', *, *, #4876, .F. ) ;
#9126 = VERTEX_POINT ( 'NONE', #11459 ) ;
#9127 = DIRECTION ( 'NONE',  ( 0.000000000000000000, 0.000000000000000000, 1.000000000000000000 ) ) ;
#9128 = CARTESIAN_POINT ( 'NONE',  ( 0.000000000000000000, 341.0487089519837696, -115.0000000000032969 ) ) ;
#9129 = AXIS2_PLACEMENT_3D ( 'NONE', #2302, #6488, #11487 ) ;
#9130 = ORIENTED_EDGE ( 'NONE', *, *, #5032, .T. ) ;
#9131 = DIRECTION ( 'NONE',  ( 0.000000000000000000, 1.000000000000000000, -0.000000000000000000 ) ) ;
#9132 = DIRECTION ( 'NONE',  ( -0.000000000000000000, -1.000000000000000000, -0.000000000000000000 ) ) ;
#9133 = ADVANCED_FACE ( 'NONE', ( #1068 ), #15332, .F. ) ;
#9134 = DIRECTION ( 'NONE',  ( 3.407805566942604354E-15, 0.9950371902099891530, -0.09950371902099955368 ) ) ;
#9135 = AXIS2_PLACEMENT_3D ( 'NONE', #14131, #2346, #15742 ) ;
#9136 = VECTOR ( 'NONE', #3948, 1000.000000000000000 ) ;
#9137 = CIRCLE ( 'NONE', #10503, 22.49999999999999645 ) ;
#9138 = FACE_OUTER_BOUND ( 'NONE', #5821, .T. ) ;
#9139 = VECTOR ( 'NONE', #5264, 1000.000000000000000 ) ;
#9140 = ORIENTED_EDGE ( 'NONE', *, *, #1631, .F. ) ;
#9141 = CARTESIAN_POINT ( 'NONE',  ( 55.99999999999989342, 549.5810598491749488, -561.6352214130889706 ) ) ;
#9142 = LINE ( 'NONE', #6452, #8592 ) ;
#9143 = EDGE_LOOP ( 'NONE', ( #7107, #7462, #5154, #16116 ) ) ;
#9144 = EDGE_CURVE ( 'NONE', #11543, #10620, #10351, .T. ) ;
#9145 = DIRECTION ( 'NONE',  ( -0.000000000000000000, -0.000000000000000000, 1.000000000000000000 ) ) ;
#9146 = ORIENTED_EDGE ( 'NONE', *, *, #786, .F. ) ;
#9147 = VECTOR ( 'NONE', #9898, 1000.000000000000000 ) ;
#9148 = DIRECTION ( 'NONE',  ( -0.9998870921963913805, -0.01502673813723916230, -0.000000000000000000 ) ) ;
#9149 = ORIENTED_EDGE ( 'NONE', *, *, #695, .F. ) ;
#9150 = CIRCLE ( 'NONE', #5027, 2.500000000000002220 ) ;
#9151 = EDGE_LOOP ( 'NONE', ( #12898, #2397, #7705, #3666, #14196, #552, #4552, #3 ) ) ;
#9152 = CARTESIAN_POINT ( 'NONE',  ( 39.41161623800082481, 323.9612906317821057, 0.000000000000000000 ) ) ;
#9153 = VECTOR ( 'NONE', #6991, 1000.000000000000000 ) ;
#9154 = DIRECTION ( 'NONE',  ( 0.000000000000000000, -0.000000000000000000, 1.000000000000000000 ) ) ;
#9155 = CARTESIAN_POINT ( 'NONE',  ( 3.324999999999999734, 12.97499999999999964, 0.000000000000000000 ) ) ;
#9156 = VERTEX_POINT ( 'NONE', #15580 ) ;
#9157 = CARTESIAN_POINT ( 'NONE',  ( 54.99999999999999289, 658.4713480608917280, -425.4301204538002139 ) ) ;
#9158 = CARTESIAN_POINT ( 'NONE',  ( 4.899999999999999467, 0.000000000000000000, 0.000000000000000000 ) ) ;
#9159 = CIRCLE ( 'NONE', #3140, 12.00000000000000178 ) ;
#9160 = EDGE_CURVE ( 'NONE', #10672, #11859, #15412, .T. ) ;
#9161 = DIRECTION ( 'NONE',  ( 0.000000000000000000, 0.000000000000000000, -1.000000000000000000 ) ) ;
#9162 = LINE ( 'NONE', #7766, #5108 ) ;
#9163 = DIRECTION ( 'NONE',  ( 1.000000000000000000, 0.000000000000000000, 0.000000000000000000 ) ) ;
#9164 = AXIS2_PLACEMENT_3D ( 'NONE', #14374, #16682, #7654 ) ;
#9165 = FACE_BOUND ( 'NONE', #11601, .T. ) ;
#9166 = AXIS2_PLACEMENT_3D ( 'NONE', #4569, #12224, #11100 ) ;
#9167 = CARTESIAN_POINT ( 'NONE',  ( 0.000000000000000000, 214.9999999999953104, -486.7326477857724853 ) ) ;
#9169 = ORIENTED_EDGE ( 'NONE', *, *, #13083, .F. ) ;
#9168 = ORIENTED_EDGE ( 'NONE', *, *, #10151, .F. ) ;
#9170 = CARTESIAN_POINT ( 'NONE',  ( -46.99999999999988631, 493.2350855268092573, -585.2659423243250103 ) ) ;
#9171 = AXIS2_PLACEMENT_3D ( 'NONE', #10443, #15851, #1520 ) ;
#9172 = CIRCLE ( 'NONE', #1775, 2.999999999999999112 ) ;
#9173 = DIRECTION ( 'NONE',  ( 0.000000000000000000, 0.000000000000000000, -1.000000000000000000 ) ) ;
#9174 = ADVANCED_FACE ( 'NONE', ( #3816 ), #12837, .F. ) ;
#9175 = CARTESIAN_POINT ( 'NONE',  ( -46.99999999999988631, 473.6663340069157471, -536.1966447803968094 ) ) ;
#9176 = DIRECTION ( 'NONE',  ( -0.000000000000000000, -1.000000000000000000, 0.000000000000000000 ) ) ;
#9177 = VERTEX_POINT ( 'NONE', #11718 ) ;
#9178 = AXIS2_PLACEMENT_3D ( 'NONE', #12810, #1042, #4975 ) ;
#9179 = FACE_OUTER_BOUND ( 'NONE', #1686, .T. ) ;
#9180 = APPLICATION_CONTEXT ( 'automotive_design' ) ;
#9181 = ADVANCED_FACE ( 'NONE', ( #8977 ), #14291, .F. ) ;
#9182 = DIRECTION ( 'NONE',  ( 0.000000000000000000, 1.000000000000000000, 0.000000000000000000 ) ) ;
#9183 = ORIENTED_EDGE ( 'NONE', *, *, #16639, .T. ) ;
#9184 = LINE ( 'NONE', #11573, #7665 ) ;
#9185 = VECTOR ( 'NONE', #3361, 1000.000000000000000 ) ;
#9186 = CARTESIAN_POINT ( 'NONE',  ( 45.00000000000000000, 515.4878487013597805, -606.7230258972047068 ) ) ;
#9187 = DIRECTION ( 'NONE',  ( 0.000000000000000000, 0.000000000000000000, -1.000000000000000000 ) ) ;
#9188 = CARTESIAN_POINT ( 'NONE',  ( 10.00000000000000000, 372.8685141053778693, -79.88019484660868841 ) ) ;
#9189 = CARTESIAN_POINT ( 'NONE',  ( 46.99999999999988631, 523.2161522479893847, -590.5524132976893270 ) ) ;
#9190 = DIRECTION ( 'NONE',  ( -0.000000000000000000, -1.000000000000000000, 0.000000000000000000 ) ) ;
#9191 = ORIENTED_EDGE ( 'NONE', *, *, #12914, .T. ) ;
#9192 = LINE ( 'NONE', #12879, #11639 ) ;
#9193 = PRODUCT_DEFINITION_FORMATION_WITH_SPECIFIED_SOURCE ( 'ANY', '', #14966, .NOT_KNOWN. ) ;
#9194 = ITEM_DEFINED_TRANSFORMATION ( 'NONE', 'NONE', #11102,  #1488 ) ;
#9195 = ADVANCED_FACE ( 'NONE', ( #15507 ), #7748, .F. ) ;
#9196 = VECTOR ( 'NONE', #12939, 1000.000000000000000 ) ;
#9197 = CARTESIAN_POINT ( 'NONE',  ( -20.00000000000003197, 3.000000000000000000, 40.00000000000000711 ) ) ;
#9198 = ORIENTED_EDGE ( 'NONE', *, *, #8374, .F. ) ;
#9199 = DIRECTION ( 'NONE',  ( 0.000000000000000000, 0.000000000000000000, 1.000000000000000000 ) ) ;
#9200 = ADVANCED_FACE ( 'NONE', ( #38 ), #16692, .F. ) ;
#9201 = LINE ( 'NONE', #13329, #2591 ) ;
#9202 = ADVANCED_FACE ( 'NONE', ( #1325 ), #8806, .T. ) ;
#9203 = EDGE_CURVE ( 'NONE', #4345, #12485, #5490, .T. ) ;
#9204 = DIRECTION ( 'NONE',  ( 1.000000000000000000, 0.000000000000000000, 8.673617379884027583E-16 ) ) ;
#9205 = ORIENTED_EDGE ( 'NONE', *, *, #4384, .F. ) ;
#9206 = LINE ( 'NONE', #11511, #12181 ) ;
#9207 = ADVANCED_FACE ( 'NONE', ( #5614 ), #9396, .T. ) ;
#9208 = FACE_OUTER_BOUND ( 'NONE', #9044, .T. ) ;
#9209 = DIRECTION ( 'NONE',  ( 0.000000000000000000, 1.000000000000000000, 0.000000000000000000 ) ) ;
#9210 = ORIENTED_EDGE ( 'NONE', *, *, #7000, .T. ) ;
#9211 = AXIS2_PLACEMENT_3D ( 'NONE', #10018, #6372, #16778 ) ;
#9212 = CARTESIAN_POINT ( 'NONE',  ( -22.99999999999999645, 68.00000000000000000, -31.00000000000005684 ) ) ;
#9213 = ORIENTED_EDGE ( 'NONE', *, *, #4192, .F. ) ;
#9214 = ORIENTED_EDGE ( 'NONE', *, *, #9354, .F. ) ;
#9215 = DIRECTION ( 'NONE',  ( -1.000000000000000000, -0.000000000000000000, -0.000000000000000000 ) ) ;
#9216 = ORIENTED_EDGE ( 'NONE', *, *, #13909, .T. ) ;
#9217 = VERTEX_POINT ( 'NONE', #13360 ) ;
#9218 = DIRECTION ( 'NONE',  ( 6.982962677686242256E-15, -6.982962677686266711E-15, 1.000000000000000000 ) ) ;
#9219 = ORIENTED_EDGE ( 'NONE', *, *, #8551, .T. ) ;
#9220 = AXIS2_PLACEMENT_3D ( 'NONE', #5069, #14522, #7722 ) ;
#9221 = ORIENTED_EDGE ( 'NONE', *, *, #15505, .T. ) ;
#9222 = AXIS2_PLACEMENT_3D ( 'NONE', #524, #14862, #4390 ) ;
#9223 = CARTESIAN_POINT ( 'NONE',  ( -25.99999999999999645, 0.000000000000000000, 40.00000000000002132 ) ) ;
#9224 = LINE ( 'NONE', #10589, #12735 ) ;
#9225 = EDGE_CURVE ( 'NONE', #13943, #14252, #1931, .T. ) ;
#9226 = VERTEX_POINT ( 'NONE', #1586 ) ;
#9227 = DIRECTION ( 'NONE',  ( 0.000000000000000000, 0.000000000000000000, 1.000000000000000000 ) ) ;
#9228 = EDGE_CURVE ( 'NONE', #11441, #14417, #8107, .T. ) ;
#9229 = CARTESIAN_POINT ( 'NONE',  ( 6.297236075819447898E-13, 187.1252973749438695, -18.71252973749450632 ) ) ;
#9230 = CARTESIAN_POINT ( 'NONE',  ( 5.162501635565829972, -12.32407335584850117, 1.509263698769704680E-15 ) ) ;
#9231 = ORIENTED_EDGE ( 'NONE', *, *, #6437, .T. ) ;
#9232 = CARTESIAN_POINT ( 'NONE',  ( 3.500000000000000000, 18.50000000000000000, 0.000000000000000000 ) ) ;
#9233 = DIRECTION ( 'NONE',  ( 0.000000000000000000, 0.000000000000000000, -1.000000000000000000 ) ) ;
#9234 = VERTEX_POINT ( 'NONE', #6803 ) ;
#9235 = CIRCLE ( 'NONE', #7565, 13.69540538389597017 ) ;
#9236 = CARTESIAN_POINT ( 'NONE',  ( 394.0000000000001137, 449.3157724647196005, -155.1251505852266632 ) ) ;
#9237 = ORIENTED_EDGE ( 'NONE', *, *, #8774, .F. ) ;
#9238 = DIRECTION ( 'NONE',  ( 1.000000000000000000, -0.000000000000000000, 0.000000000000000000 ) ) ;
#9239 = EDGE_LOOP ( 'NONE', ( #5353, #6980, #15359, #3275 ) ) ;
#9240 = ORIENTED_EDGE ( 'NONE', *, *, #12106, .F. ) ;
#9241 = CARTESIAN_POINT ( 'NONE',  ( 4.469960816887838430E-15, 26.00000000000000000, 36.50000000000000000 ) ) ;
#9242 = DIRECTION ( 'NONE',  ( 0.000000000000000000, 0.000000000000000000, -1.000000000000000000 ) ) ;
#9243 = DIRECTION ( 'NONE',  ( 0.000000000000000000, -1.000000000000000000, 0.000000000000000000 ) ) ;
#9244 = CIRCLE ( 'NONE', #13358, 2.500000000000002220 ) ;
#9245 = ORIENTED_EDGE ( 'NONE', *, *, #1523, .F. ) ;
#9246 = VECTOR ( 'NONE', #15904, 1000.000000000000000 ) ;
#9247 = DIRECTION ( 'NONE',  ( 1.000000000000000000, -0.000000000000000000, 0.000000000000000000 ) ) ;
#9248 = FACE_OUTER_BOUND ( 'NONE', #2389, .T. ) ;
#9249 = CARTESIAN_POINT ( 'NONE',  ( -35.00000000000000000, 19.00000000000000000, 20.99999999999999289 ) ) ;
#9250 = DIRECTION ( 'NONE',  ( 1.000000000000000000, -0.000000000000000000, -0.000000000000000000 ) ) ;
#9251 = CARTESIAN_POINT ( 'NONE',  ( -49.99999999999999289, 515.4878487013597805, -546.7230258972048205 ) ) ;
#9252 = LINE ( 'NONE', #5372, #15204 ) ;
#9253 = CARTESIAN_POINT ( 'NONE',  ( 22.99999999999998224, 10.00000000000000000, -31.99999999999998579 ) ) ;
#9255 = ORIENTED_EDGE ( 'NONE', *, *, #15185, .T. ) ;
#9254 = VERTEX_POINT ( 'NONE', #12062 ) ;
#9256 = AXIS2_PLACEMENT_3D ( 'NONE', #12329, #4520, #11126 ) ;
#9257 = DIRECTION ( 'NONE',  ( 0.000000000000000000, 0.000000000000000000, -1.000000000000000000 ) ) ;
#9258 = CARTESIAN_POINT ( 'NONE',  ( 0.03302700000128662439, 285.4366476906504317, 37.52989836422092651 ) ) ;
#9259 = DIRECTION ( 'NONE',  ( 1.000000000000000000, 0.000000000000000000, 0.000000000000000000 ) ) ;
#9260 = DIRECTION ( 'NONE',  ( 1.000000000000000000, -0.000000000000000000, 0.000000000000000000 ) ) ;
#9261 = ORIENTED_EDGE ( 'NONE', *, *, #7318, .T. ) ;
#9262 = CARTESIAN_POINT ( 'NONE',  ( -55.99999999999989342, 523.2161522479893847, -590.5524132976893270 ) ) ;
#9263 = AXIS2_PLACEMENT_3D ( 'NONE', #2473, #12958, #13219 ) ;
#9264 = CARTESIAN_POINT ( 'NONE',  ( 47.50000000000000000, 196.3050121726289206, -75.00000000000000000 ) ) ;
#9265 = EDGE_LOOP ( 'NONE', ( #12083, #6831 ) ) ;
#9266 = CARTESIAN_POINT ( 'NONE',  ( 10.00000000000000000, 381.0487089519826895, 2.719601036885452502E-12 ) ) ;
#9267 = LINE ( 'NONE', #15540, #16349 ) ;
#9268 = CARTESIAN_POINT ( 'NONE',  ( -36.00000000000000711, 10.00000000000000000, -22.00000000000000355 ) ) ;
#9269 = ADVANCED_FACE ( 'NONE', ( #301, #5518, #16004 ), #8191, .F. ) ;
#9270 = CARTESIAN_POINT ( 'NONE',  ( -6.117449311278470645E-17, 355.3192028797624857, -29.71049682360898814 ) ) ;
#9271 = DIRECTION ( 'NONE',  ( 0.000000000000000000, 0.000000000000000000, -1.000000000000000000 ) ) ;
#9272 = ORIENTED_EDGE ( 'NONE', *, *, #59, .T. ) ;
#9273 = CARTESIAN_POINT ( 'NONE',  ( -37.00000000000000711, 6.000000000000000000, -23.00000000000000000 ) ) ;
#9274 = EDGE_CURVE ( 'NONE', #5350, #9290, #2197, .T. ) ;
#9275 = AXIS2_PLACEMENT_3D ( 'NONE', #7979, #1559, #12116 ) ;
#9276 = DIRECTION ( 'NONE',  ( 1.000000000000000000, -0.000000000000000000, 0.000000000000000000 ) ) ;
#9277 = VERTEX_POINT ( 'NONE', #389 ) ;
#9278 = CARTESIAN_POINT ( 'NONE',  ( 35.00000000000000711, 8.000000000000000000, -21.00000000000000355 ) ) ;
#9279 = CARTESIAN_POINT ( 'NONE',  ( -3.270000000000000462, 218.4499468633019603, 287.1312267635915987 ) ) ;
#9280 = DIRECTION ( 'NONE',  ( 0.000000000000000000, -0.6366988521258363232, 0.7711125544961918710 ) ) ;
#9281 = ORIENTED_EDGE ( 'NONE', *, *, #10864, .T. ) ;
#9282 = LINE ( 'NONE', #3011, #8876 ) ;
#9283 = CARTESIAN_POINT ( 'NONE',  ( 4.286263797015737285E-15, 0.000000000000000000, -35.00000000000000711 ) ) ;
#9284 = PLANE ( 'NONE',  #5123 ) ;
#9285 = ORIENTED_EDGE ( 'NONE', *, *, #13841, .F. ) ;
#9286 = EDGE_CURVE ( 'NONE', #5261, #13502, #10857, .T. ) ;
#9287 = VECTOR ( 'NONE', #5795, 1000.000000000000000 ) ;
#9288 = PRESENTATION_STYLE_ASSIGNMENT (( #6599 ) ) ;
#9289 = ORIENTED_EDGE ( 'NONE', *, *, #6659, .F. ) ;
#9290 = VERTEX_POINT ( 'NONE', #14553 ) ;
#9291 = DIRECTION ( 'NONE',  ( -0.000000000000000000, 0.000000000000000000, 1.000000000000000000 ) ) ;
#9292 = ORIENTED_EDGE ( 'NONE', *, *, #15166, .F. ) ;
#9293 = EDGE_CURVE ( 'NONE', #1294, #16266, #7954, .T. ) ;
#9294 = DIRECTION ( 'NONE',  ( 1.000000000000000000, 0.000000000000000000, 0.000000000000000000 ) ) ;
#9295 = EDGE_CURVE ( 'NONE', #5350, #11430, #10161, .T. ) ;
#9296 = ADVANCED_FACE ( 'NONE', ( #13180 ), #1406, .T. ) ;
#9297 = ORIENTED_EDGE ( 'NONE', *, *, #9008, .F. ) ;
#9298 = ORIENTED_EDGE ( 'NONE', *, *, #4262, .T. ) ;
#9299 = DIRECTION ( 'NONE',  ( -0.000000000000000000, -0.000000000000000000, 1.000000000000000000 ) ) ;
#9300 = PRODUCT_DEFINITION_CONTEXT ( 'detailed design', #13243, 'design' ) ;
#9301 = CARTESIAN_POINT ( 'NONE',  ( -32.00000000000000711, 6.000000000000000000, -22.00000000000000355 ) ) ;
#9302 = ORIENTED_EDGE ( 'NONE', *, *, #14773, .T. ) ;
#9303 = CARTESIAN_POINT ( 'NONE',  ( 0.000000000000000000, 309.2289037985890445, -146.8198051533984199 ) ) ;
#9304 = DIRECTION ( 'NONE',  ( -1.000000000000000000, 0.000000000000000000, 0.000000000000000000 ) ) ;
#9305 = VERTEX_POINT ( 'NONE', #9312 ) ;
#9306 = AXIS2_PLACEMENT_3D ( 'NONE', #6385, #7598, #11395 ) ;
#9307 = LINE ( 'NONE', #14544, #6388 ) ;
#9308 = ORIENTED_EDGE ( 'NONE', *, *, #12525, .T. ) ;
#9309 = CARTESIAN_POINT ( 'NONE',  ( 0.000000000000000000, 23.00000000000000000, -34.00000000000000000 ) ) ;
#9310 = FACE_OUTER_BOUND ( 'NONE', #5151, .T. ) ;
#9311 = ORIENTED_EDGE ( 'NONE', *, *, #6011, .F. ) ;
#9312 = CARTESIAN_POINT ( 'NONE',  ( 22.99999999999998224, 10.00000000000000000, 37.00000000000000711 ) ) ;
#9313 = ORIENTED_EDGE ( 'NONE', *, *, #1102, .T. ) ;
#9314 = ADVANCED_FACE ( 'NONE', ( #2777 ), #5355, .F. ) ;
#9315 = EDGE_CURVE ( 'NONE', #4609, #4810, #12, .T. ) ;
#9316 = CARTESIAN_POINT ( 'NONE',  ( 39.06972645625037899, 346.7108172824755457, 0.000000000000000000 ) ) ;
#9317 = EDGE_CURVE ( 'NONE', #4921, #16177, #7635, .T. ) ;
#9318 = VERTEX_POINT ( 'NONE', #10478 ) ;
#9319 = VECTOR ( 'NONE', #15276, 1000.000000000000000 ) ;
#9320 = ORIENTED_EDGE ( 'NONE', *, *, #7309, .F. ) ;
#9321 = CARTESIAN_POINT ( 'NONE',  ( 1.574999999999999956, 14.92500000000000071, 0.000000000000000000 ) ) ;
#9322 = DIRECTION ( 'NONE',  ( 0.000000000000000000, 0.09950371902098545385, -0.9950371902099903743 ) ) ;
#9323 = PLANE ( 'NONE',  #9980 ) ;
#9324 = ORIENTED_EDGE ( 'NONE', *, *, #7072, .F. ) ;
#9325 = FACE_OUTER_BOUND ( 'NONE', #13790, .T. ) ;
#9326 = PRODUCT_DEFINITION_SHAPE ( 'NONE', 'NONE',  #16978 ) ;
#9327 = CARTESIAN_POINT ( 'NONE',  ( 4.025000000000000355, 0.000000000000000000, 0.000000000000000000 ) ) ;
#9328 = CARTESIAN_POINT ( 'NONE',  ( 10.00000000000000000, 620.7506394335853201, -11.00000000000000000 ) ) ;
#9329 = DIRECTION ( 'NONE',  ( -0.000000000000000000, -0.000000000000000000, 1.000000000000000000 ) ) ;
#9330 = CARTESIAN_POINT ( 'NONE',  ( -33.99999999999997158, -20.00000000000000000, -25.99999999999999645 ) ) ;
#9331 = CIRCLE ( 'NONE', #7118, 3.300000000000004263 ) ;
#9332 = AXIS2_PLACEMENT_3D ( 'NONE', #12684, #16876, #923 ) ;
#9333 = DIRECTION ( 'NONE',  ( 0.000000000000000000, 0.000000000000000000, -1.000000000000000000 ) ) ;
#9334 =( NAMED_UNIT ( * ) PLANE_ANGLE_UNIT ( ) SI_UNIT ( $, .RADIAN. ) );
#9336 = EDGE_LOOP ( 'NONE', ( #774, #15089, #5067, #8372 ) ) ;
#9335 = ORIENTED_EDGE ( 'NONE', *, *, #7526, .F. ) ;
#9337 = CARTESIAN_POINT ( 'NONE',  ( 36.99999999999999289, 0.000000000000000000, 22.99999999999999645 ) ) ;
#9338 = LINE ( 'NONE', #6663, #56 ) ;
#9339 = CARTESIAN_POINT ( 'NONE',  ( 46.99999999999988631, 549.5810598491746077, -518.1154249974242703 ) ) ;
#9340 = FACE_OUTER_BOUND ( 'NONE', #15106, .T. ) ;
#9341 = ORIENTED_EDGE ( 'NONE', *, *, #7700, .T. ) ;
#9342 = AXIS2_PLACEMENT_3D ( 'NONE', #6817, #14486, #13458 ) ;
#9343 = DIRECTION ( 'NONE',  ( 0.000000000000000000, 0.000000000000000000, 1.000000000000000000 ) ) ;
#9344 = DIRECTION ( 'NONE',  ( 0.000000000000000000, 1.000000000000000000, 0.000000000000000000 ) ) ;
#9345 = ORIENTED_EDGE ( 'NONE', *, *, #14921, .F. ) ;
#9346 = DIRECTION ( 'NONE',  ( 0.000000000000000000, -7.137148015447440312E-15, 1.000000000000000000 ) ) ;
#9347 = ADVANCED_FACE ( 'NONE', ( #9028 ), #6339, .T. ) ;
#9348 = CYLINDRICAL_SURFACE ( 'NONE', #2645, 59.99999999999994316 ) ;
#9349 = LINE ( 'NONE', #15953, #8277 ) ;
#9350 = DIRECTION ( 'NONE',  ( 0.000000000000000000, 0.000000000000000000, 1.000000000000000000 ) ) ;
#9351 = FILL_AREA_STYLE_COLOUR ( '', #11734 ) ;
#9352 = ORIENTED_EDGE ( 'NONE', *, *, #10313, .T. ) ;
#9353 = VECTOR ( 'NONE', #12087, 1000.000000000000000 ) ;
#9354 = EDGE_CURVE ( 'NONE', #8101, #6054, #4128, .T. ) ;
#9355 = CARTESIAN_POINT ( 'NONE',  ( 55.99999999999989342, 493.2350855268092573, -585.2659423243250103 ) ) ;
#9356 = SHAPE_REPRESENTATION ( 'Assem2', ( #1780, #408, #11922, #12474 ), #684 ) ;
#9357 = DIRECTION ( 'NONE',  ( 0.000000000000000000, 0.3746065934157932764, 0.9271838545668352749 ) ) ;
#9358 = DIRECTION ( 'NONE',  ( -3.854941057726255847E-16, -0.000000000000000000, 1.000000000000000000 ) ) ;
#9359 = ORIENTED_EDGE ( 'NONE', *, *, #12907, .T. ) ;
#9360 = DIRECTION ( 'NONE',  ( -0.000000000000000000, -1.000000000000000000, -0.000000000000000000 ) ) ;
#9361 = LINE ( 'NONE', #6854, #16581 ) ;
#9362 = AXIS2_PLACEMENT_3D ( 'NONE', #12245, #13537, #4512 ) ;
#9363 = DIRECTION ( 'NONE',  ( 3.854941057726254367E-16, 0.000000000000000000, 1.000000000000000000 ) ) ;
#9364 = ORIENTED_EDGE ( 'NONE', *, *, #13100, .F. ) ;
#9365 = CARTESIAN_POINT ( 'NONE',  ( 10.00000000000000000, 306.0487089519832011, -80.00000000000380851 ) ) ;
#9366 = LINE ( 'NONE', #2839, #9009 ) ;
#9367 = FACE_OUTER_BOUND ( 'NONE', #9825, .T. ) ;
#9368 = EDGE_LOOP ( 'NONE', ( #13098, #9146, #2041, #6860 ) ) ;
#9369 = ADVANCED_FACE ( 'NONE', ( #11594, #2661 ), #1213, .T. ) ;
#9370 = CLOSED_SHELL ( 'NONE', ( #6946, #11567, #14856, #10272, #9799, #14309, #7582, #13300, #791, #16506, #10450, #13699, #4824, #10452, #12035, #918, #1096, #6871, #10895, #2262, #1020, #10555, #14928, #6298, #1856, #285, #9207, #6536, #3056, #14977, #5313, #3947, #5522, #11281, #8987, #1752, #4494, #10124 ) ) ;
#9371 =( NAMED_UNIT ( * ) SI_UNIT ( $, .STERADIAN. ) SOLID_ANGLE_UNIT ( ) );
#9372 = ORIENTED_EDGE ( 'NONE', *, *, #16956, .F. ) ;
#9373 = ORIENTED_EDGE ( 'NONE', *, *, #8897, .T. ) ;
#9374 = CARTESIAN_POINT ( 'NONE',  ( -31.00000000000005684, 0.000000000000000000, 23.00000000000000355 ) ) ;
#9375 = VERTEX_POINT ( 'NONE', #5144 ) ;
#9376 = APPLICATION_PROTOCOL_DEFINITION ( 'draft international standard', 'automotive_design', 1998, #7958 ) ;
#9377 = VECTOR ( 'NONE', #3205, 1000.000000000000000 ) ;
#9378 = ORIENTED_EDGE ( 'NONE', *, *, #4583, .F. ) ;
#9379 = AXIS2_PLACEMENT_3D ( 'NONE', #3781, #5136, #7625 ) ;
#9380 = VERTEX_POINT ( 'NONE', #9111 ) ;
#9381 = EDGE_CURVE ( 'NONE', #9254, #6128, #16746, .T. ) ;
#9382 = AXIS2_PLACEMENT_3D ( 'NONE', #11544, #16947, #4931 ) ;
#9383 = DIRECTION ( 'NONE',  ( 0.000000000000000000, 0.000000000000000000, 1.000000000000000000 ) ) ;
#9384 = EDGE_CURVE ( 'NONE', #16924, #16617, #14186, .T. ) ;
#9385 = DIRECTION ( 'NONE',  ( 0.000000000000000000, 1.000000000000000000, 0.000000000000000000 ) ) ;
#9386 = ORIENTED_EDGE ( 'NONE', *, *, #5403, .F. ) ;
#9387 = CARTESIAN_POINT ( 'NONE',  ( -23.00000000000002132, 10.00000000000000000, 32.00000000000000000 ) ) ;
#9388 = CARTESIAN_POINT ( 'NONE',  ( 39.41161623800082481, 323.9612906317821057, -6.736600000000000144 ) ) ;
#9389 = ORIENTED_EDGE ( 'NONE', *, *, #5576, .F. ) ;
#9390 = EDGE_CURVE ( 'NONE', #3466, #8101, #2753, .T. ) ;
#9391 = DIRECTION ( 'NONE',  ( 0.000000000000000000, 0.000000000000000000, 1.000000000000000000 ) ) ;
#9392 = ORIENTED_EDGE ( 'NONE', *, *, #1502, .F. ) ;
#9393 = FACE_OUTER_BOUND ( 'NONE', #12905, .T. ) ;
#9394 = FACE_OUTER_BOUND ( 'NONE', #1226, .T. ) ;
#9395 = ORIENTED_EDGE ( 'NONE', *, *, #1342, .T. ) ;
#9396 = PLANE ( 'NONE',  #6026 ) ;
#9397 = ORIENTED_EDGE ( 'NONE', *, *, #897, .F. ) ;
#9398 = CARTESIAN_POINT ( 'NONE',  ( 22.99999999999995737, 3.000000000000000000, -33.99999999999998579 ) ) ;
#9399 = ORIENTED_EDGE ( 'NONE', *, *, #9488, .F. ) ;
#9400 = CIRCLE ( 'NONE', #6100, 3.000000000000002665 ) ;
#9401 = ORIENTED_EDGE ( 'NONE', *, *, #3050, .F. ) ;
#9402 = EDGE_CURVE ( 'NONE', #13502, #6506, #6299, .T. ) ;
#9403 = DIRECTION ( 'NONE',  ( -1.000000000000000000, 0.000000000000000000, -0.000000000000000000 ) ) ;
#9404 = CARTESIAN_POINT ( 'NONE',  ( 0.000000000000000000, -3.000000000000000000, 0.000000000000000000 ) ) ;
#9405 = VECTOR ( 'NONE', #1927, 1000.000000000000000 ) ;
#9406 = ORIENTED_EDGE ( 'NONE', *, *, #7925, .T. ) ;
#9407 = CARTESIAN_POINT ( 'NONE',  ( 0.000000000000000000, 19.00100000000000122, -18.50000000000000000 ) ) ;
#9408 = VECTOR ( 'NONE', #8105, 1000.000000000000227 ) ;
#9409 = AXIS2_PLACEMENT_3D ( 'NONE', #1963, #773, #852 ) ;
#9410 = CARTESIAN_POINT ( 'NONE',  ( -3.000000000000002220, 60.00000000000000711, 6.000000000000000000 ) ) ;
#9411 = EDGE_CURVE ( 'NONE', #10513, #15829, #15917, .T. ) ;
#9412 = ADVANCED_FACE ( 'NONE', ( #16828 ), #1122, .F. ) ;
#9413 = EDGE_CURVE ( 'NONE', #8924, #6167, #4937, .T. ) ;
#9414 = DIRECTION ( 'NONE',  ( -0.000000000000000000, -0.000000000000000000, 1.000000000000000000 ) ) ;
#9415 = EDGE_CURVE ( 'NONE', #16577, #15508, #5323, .T. ) ;
#9416 = DIRECTION ( 'NONE',  ( 0.000000000000000000, 0.000000000000000000, 1.000000000000000000 ) ) ;
#9417 = DIRECTION ( 'NONE',  ( 0.000000000000000000, -0.000000000000000000, 1.000000000000000000 ) ) ;
#9418 = DIRECTION ( 'NONE',  ( 0.000000000000000000, 0.000000000000000000, 1.000000000000000000 ) ) ;
#9419 = CIRCLE ( 'NONE', #9695, 18.49999999999998934 ) ;
#9420 = DIRECTION ( 'NONE',  ( 1.000000000000000000, -0.000000000000000000, 0.000000000000000000 ) ) ;
#9421 = CARTESIAN_POINT ( 'NONE',  ( -55.99999999999989342, 493.2350855268092573, -585.2659423243250103 ) ) ;
#9423 = VERTEX_POINT ( 'NONE', #6 ) ;
#9422 = ORIENTED_EDGE ( 'NONE', *, *, #10248, .F. ) ;
#9424 = CARTESIAN_POINT ( 'NONE',  ( 46.99999999999988631, 493.2350855268092573, -580.5705369404290650 ) ) ;
#9425 = VECTOR ( 'NONE', #3306, 1000.000000000000114 ) ;
#9426 = VECTOR ( 'NONE', #12845, 1000.000000000000000 ) ;
#9427 = CARTESIAN_POINT ( 'NONE',  ( -1.281199806755545456, 288.9467639778928856, 37.61247111518799358 ) ) ;
#9428 = CARTESIAN_POINT ( 'NONE',  ( -40.00000000000000711, 10.00000000000000000, -26.00000000000000000 ) ) ;
#9429 = PLANE ( 'NONE',  #913 ) ;
#9430 = VECTOR ( 'NONE', #10998, 1000.000000000000000 ) ;
#9431 = VERTEX_POINT ( 'NONE', #15630 ) ;
#9432 = DIRECTION ( 'NONE',  ( 0.000000000000000000, 0.000000000000000000, 1.000000000000000000 ) ) ;
#9433 = STYLED_ITEM ( 'NONE', ( #9288 ), #3006 ) ;
#9434 = AXIS2_PLACEMENT_3D ( 'NONE', #12883, #11844, #12965 ) ;
#9435 = CARTESIAN_POINT ( 'NONE',  ( -36.00000000000000711, 6.000000000000000000, -22.00000000000000355 ) ) ;
#9436 = ORIENTED_EDGE ( 'NONE', *, *, #5280, .T. ) ;
#9437 = CARTESIAN_POINT ( 'NONE',  ( 31.81980515339464333, 11.00000000000000000, -28.51980515339463906 ) ) ;
#9438 = EDGE_CURVE ( 'NONE', #16577, #6651, #1293, .T. ) ;
#9439 = VECTOR ( 'NONE', #7069, 1000.000000000000000 ) ;
#9440 = CARTESIAN_POINT ( 'NONE',  ( 21.99999999999998224, 8.000000000000000000, -32.99999999999999289 ) ) ;
#9441 = FACE_OUTER_BOUND ( 'NONE', #13426, .T. ) ;
#9442 = AXIS2_PLACEMENT_3D ( 'NONE', #14403, #11997, #7858 ) ;
#9443 = DIRECTION ( 'NONE',  ( -1.000000000000000000, 0.000000000000000000, -0.000000000000000000 ) ) ;
#9444 = CARTESIAN_POINT ( 'NONE',  ( 0.000000000000000000, 620.7506394335853201, 305.2562418976663707 ) ) ;
#9445 = ORIENTED_EDGE ( 'NONE', *, *, #3427, .T. ) ;
#9446 = DIRECTION ( 'NONE',  ( 0.000000000000000000, 0.000000000000000000, 1.000000000000000000 ) ) ;
#9447 = CONTEXT_DEPENDENT_SHAPE_REPRESENTATION ( #7855, #16331 ) ;
#9448 = MECHANICAL_DESIGN_GEOMETRIC_PRESENTATION_REPRESENTATION (  '', ( #3955 ), #15735 ) ;
#9449 = CARTESIAN_POINT ( 'NONE',  ( 394.0000000000001137, 449.3157724647197142, 33.76061909850716347 ) ) ;
#9450 = VECTOR ( 'NONE', #13165, 1000.000000000000000 ) ;
#9451 = CARTESIAN_POINT ( 'NONE',  ( 46.99999999999988631, 493.2350855268086320, -494.4847040861889127 ) ) ;
#9452 = ORIENTED_EDGE ( 'NONE', *, *, #3232, .F. ) ;
#9453 = CIRCLE ( 'NONE', #16037, 25.25038683781155413 ) ;
#9454 = DIRECTION ( 'NONE',  ( 0.000000000000000000, 0.000000000000000000, -1.000000000000000000 ) ) ;
#9455 = PRODUCT_DEFINITION_CONTEXT ( 'detailed design', #2937, 'design' ) ;
#9456 = FACE_OUTER_BOUND ( 'NONE', #3639, .T. ) ;
#9457 = CARTESIAN_POINT ( 'NONE',  ( 55.99999999999989342, 523.2161522479893847, -576.8570079137933817 ) ) ;
#9458 = ORIENTED_EDGE ( 'NONE', *, *, #4060, .T. ) ;
#9459 = DIRECTION ( 'NONE',  ( 1.000000000000000000, 0.000000000000000000, 0.000000000000000000 ) ) ;
#9460 = DIRECTION ( 'NONE',  ( -0.000000000000000000, -1.000000000000000000, 0.000000000000000000 ) ) ;
#9461 = CARTESIAN_POINT ( 'NONE',  ( 0.000000000000000000, 339.3157724647196005, -110.6822657433597925 ) ) ;
#9462 = ORIENTED_EDGE ( 'NONE', *, *, #2919, .F. ) ;
#9463 = VECTOR ( 'NONE', #344, 1000.000000000000000 ) ;
#9464 = DIRECTION ( 'NONE',  ( -0.000000000000000000, -1.000000000000000000, 0.000000000000000000 ) ) ;
#9465 = AXIS2_PLACEMENT_3D ( 'NONE', #15343, #3496, #13888 ) ;
#9466 = ORIENTED_EDGE ( 'NONE', *, *, #16845, .F. ) ;
#9467 = ORIENTED_EDGE ( 'NONE', *, *, #10367, .T. ) ;
#9468 = CARTESIAN_POINT ( 'NONE',  ( 21.00000000000000000, 19.00000000000000000, 35.00000000000001421 ) ) ;
#9469 = AXIS2_PLACEMENT_3D ( 'NONE', #6586, #5396, #14595 ) ;
#9470 = EDGE_LOOP ( 'NONE', ( #2688, #4406, #6885, #1915 ) ) ;
#9471 = AXIS2_PLACEMENT_3D ( 'NONE', #2204, #6228, #7681 ) ;
#9472 = EDGE_CURVE ( 'NONE', #5278, #3550, #837, .T. ) ;
#9473 = PRODUCT_DEFINITION_SHAPE ( 'NONE', 'NONE',  #16966 ) ;
#9474 = ORIENTED_EDGE ( 'NONE', *, *, #1206, .T. ) ;
#9475 = ORIENTED_EDGE ( 'NONE', *, *, #6507, .T. ) ;
#9476 = DIRECTION ( 'NONE',  ( 0.000000000000000000, 1.000000000000000000, 0.000000000000000000 ) ) ;
#9477 = CARTESIAN_POINT ( 'NONE',  ( -55.99999999999989342, 493.2350855268086320, -503.4847040861888559 ) ) ;
#9478 = EDGE_LOOP ( 'NONE', ( #1100, #14645 ) ) ;
#9479 = AXIS2_PLACEMENT_3D ( 'NONE', #6288, #16620, #7751 ) ;
#9480 = DIRECTION ( 'NONE',  ( -0.000000000000000000, -1.000000000000000000, -0.000000000000000000 ) ) ;
#9481 = CARTESIAN_POINT ( 'NONE',  ( 54.99999999999999289, 515.4878487013597805, -546.7230258972048205 ) ) ;
#9482 = ORIENTED_EDGE ( 'NONE', *, *, #6489, .F. ) ;
#9483 = CARTESIAN_POINT ( 'NONE',  ( -45.00000000000000000, 473.6663340069157471, -531.5012393965008641 ) ) ;
#9484 = VERTEX_POINT ( 'NONE', #6258 ) ;
#9485 = CARTESIAN_POINT ( 'NONE',  ( 34.00000000000002842, -20.00000000000000000, 23.00000000000000355 ) ) ;
#9486 = CARTESIAN_POINT ( 'NONE',  ( 5.945602903476760126, -13.89560290347679938, -1.701720561796553076E-15 ) ) ;
#9487 = ORIENTED_EDGE ( 'NONE', *, *, #7700, .F. ) ;
#9488 = EDGE_CURVE ( 'NONE', #6283, #5074, #11509, .T. ) ;
#9489 = EDGE_CURVE ( 'NONE', #9234, #1606, #15715, .T. ) ;
#9490 = DIRECTION ( 'NONE',  ( -1.000000000000000000, 0.000000000000000000, -0.000000000000000000 ) ) ;
#9491 = ORIENTED_EDGE ( 'NONE', *, *, #8132, .T. ) ;
#9493 = LINE ( 'NONE', #9316, #1256 ) ;
#9492 = AXIS2_PLACEMENT_3D ( 'NONE', #376, #5605, #13762 ) ;
#9494 = TOROIDAL_SURFACE ( 'NONE', #14428, 4.695405383895982609, 9.000000000000000000 ) ;
#9495 = VERTEX_POINT ( 'NONE', #10229 ) ;
#9496 = ADVANCED_FACE ( 'NONE', ( #3709 ), #2404, .F. ) ;
#9497 = ORIENTED_EDGE ( 'NONE', *, *, #16956, .T. ) ;
#9498 = PLANE ( 'NONE',  #11854 ) ;
#9499 = LINE ( 'NONE', #14738, #15655 ) ;
#9500 = CARTESIAN_POINT ( 'NONE',  ( 5.941205806953520074, 0.000000000000000000, 0.000000000000000000 ) ) ;
#9501 = CARTESIAN_POINT ( 'NONE',  ( -2.220446049250313081E-13, 135.5000000000000000, 3.000000000000000000 ) ) ;
#9502 = DIRECTION ( 'NONE',  ( 0.000000000000000000, -0.000000000000000000, -1.000000000000000000 ) ) ;
#9503 = VECTOR ( 'NONE', #12037, 1000.000000000000114 ) ;
#9504 = PLANE ( 'NONE',  #7099 ) ;
#9505 = CIRCLE ( 'NONE', #4567, 3.000000000000000000 ) ;
#9506 = DIRECTION ( 'NONE',  ( 0.000000000000000000, 0.000000000000000000, -1.000000000000000000 ) ) ;
#9507 = LINE ( 'NONE', #2885, #7849 ) ;
#9508 = LINE ( 'NONE', #15933, #6917 ) ;
#9509 = EDGE_CURVE ( 'NONE', #13438, #9059, #12005, .T. ) ;
#9510 = CARTESIAN_POINT ( 'NONE',  ( 1.250085104875786612E-12, 218.4499468633019603, 287.1312267635915987 ) ) ;
#9511 = CARTESIAN_POINT ( 'NONE',  ( -45.00000000000000000, 515.4878487013597805, -486.7230258972047636 ) ) ;
#9513 = ORIENTED_EDGE ( 'NONE', *, *, #1107, .T. ) ;
#9512 = EDGE_LOOP ( 'NONE', ( #13891, #7515, #14580, #1033 ) ) ;
#9514 = FACE_OUTER_BOUND ( 'NONE', #14447, .T. ) ;
#9515 = EDGE_CURVE ( 'NONE', #16501, #16504, #10142, .T. ) ;
#9516 = EDGE_CURVE ( 'NONE', #12617, #16287, #12104, .T. ) ;
#9517 = CIRCLE ( 'NONE', #6747, 18.50000000000000000 ) ;
#9518 = EDGE_CURVE ( 'NONE', #2662, #7189, #7868, .T. ) ;
#9519 = CARTESIAN_POINT ( 'NONE',  ( -3.197567832866743398, 286.4953233758678834, 37.56865621330340588 ) ) ;
#9520 = AXIS2_PLACEMENT_3D ( 'NONE', #7914, #14056, #1398 ) ;
#9521 = ADVANCED_FACE ( 'NONE', ( #14410 ), #2808, .F. ) ;
#9522 = DIRECTION ( 'NONE',  ( 0.000000000000000000, 0.000000000000000000, 1.000000000000000000 ) ) ;
#9523 = DIRECTION ( 'NONE',  ( -1.000000000000000000, -0.000000000000000000, -0.000000000000000000 ) ) ;
#9524 = VERTEX_POINT ( 'NONE', #10540 ) ;
#9525 = CARTESIAN_POINT ( 'NONE',  ( 37.18009836720079875, 352.3758082234937206, 0.000000000000000000 ) ) ;
#9526 = CARTESIAN_POINT ( 'NONE',  ( 0.000000000000000000, 620.7506394335853201, 109.9999999999999858 ) ) ;
#9527 = ORIENTED_EDGE ( 'NONE', *, *, #13100, .T. ) ;
#9528 = DIRECTION ( 'NONE',  ( -1.000000000000000000, 0.000000000000000000, -0.000000000000000000 ) ) ;
#9529 = CARTESIAN_POINT ( 'NONE',  ( 30.99999999999997513, 0.000000000000000000, 25.99999999999999645 ) ) ;
#9530 = DIRECTION ( 'NONE',  ( 0.000000000000000000, 1.000000000000000000, 0.000000000000000000 ) ) ;
#9531 = AXIS2_PLACEMENT_3D ( 'NONE', #6908, #148, #8030 ) ;
#9532 =( NAMED_UNIT ( * ) PLANE_ANGLE_UNIT ( ) SI_UNIT ( $, .RADIAN. ) );
#9533 = DIRECTION ( 'NONE',  ( 0.000000000000000000, 0.000000000000000000, -1.000000000000000000 ) ) ;
#9534 = CYLINDRICAL_SURFACE ( 'NONE', #11299, 35.00000000000000711 ) ;
#9535 = ORIENTED_EDGE ( 'NONE', *, *, #5916, .T. ) ;
#9536 = DIRECTION ( 'NONE',  ( 0.000000000000000000, 0.000000000000000000, 1.000000000000000000 ) ) ;
#9537 = EDGE_CURVE ( 'NONE', #5722, #1188, #9905, .T. ) ;
#9538 = EDGE_CURVE ( 'NONE', #10225, #11540, #15857, .T. ) ;
#9539 = DIRECTION ( 'NONE',  ( -1.000000000000000000, -0.000000000000000000, -0.000000000000000000 ) ) ;
#9540 = ADVANCED_FACE ( 'NONE', ( #5197 ), #2549, .F. ) ;
#9541 = VECTOR ( 'NONE', #11756, 1000.000000000000000 ) ;
#9542 = ORIENTED_EDGE ( 'NONE', *, *, #758, .T. ) ;
#9543 = DIRECTION ( 'NONE',  ( 0.000000000000000000, -0.9950371902099902632, 0.09950371902098713306 ) ) ;
#9544 = DIRECTION ( 'NONE',  ( 0.000000000000000000, 1.000000000000000000, 0.000000000000000000 ) ) ;
#9545 = PLANE ( 'NONE',  #2905 ) ;
#9546 = VERTEX_POINT ( 'NONE', #12723 ) ;
#9547 = CARTESIAN_POINT ( 'NONE',  ( 55.99999999999989342, 473.6663340069157471, -536.1966447803968094 ) ) ;
#9548 = LINE ( 'NONE', #11855, #3795 ) ;
#9549 = DIRECTION ( 'NONE',  ( -0.000000000000000000, 0.000000000000000000, -1.000000000000000000 ) ) ;
#9550 = ORIENTED_EDGE ( 'NONE', *, *, #4992, .T. ) ;
#9551 = EDGE_CURVE ( 'NONE', #2249, #5942, #11538, .T. ) ;
#9552 = ORIENTED_EDGE ( 'NONE', *, *, #11904, .T. ) ;
#9553 = ORIENTED_EDGE ( 'NONE', *, *, #2130, .T. ) ;
#9554 = VECTOR ( 'NONE', #9866, 1000.000000000000000 ) ;
#9555 = CARTESIAN_POINT ( 'NONE',  ( 1.399999999999999911, -13.62500000000000000, -1.668581263838268760E-15 ) ) ;
#9556 = AXIS2_PLACEMENT_3D ( 'NONE', #13778, #10086, #9914 ) ;
#9557 = ORIENTED_EDGE ( 'NONE', *, *, #8064, .F. ) ;
#9558 = APPLICATION_PROTOCOL_DEFINITION ( 'draft international standard', 'automotive_design', 1998, #2147 ) ;
#9559 = ORIENTED_EDGE ( 'NONE', *, *, #7590, .T. ) ;
#9560 = ORIENTED_EDGE ( 'NONE', *, *, #5969, .F. ) ;
#9561 = CARTESIAN_POINT ( 'NONE',  ( 0.000000000000000000, 341.0487089519837696, -133.5000000000032969 ) ) ;
#9562 = CARTESIAN_POINT ( 'NONE',  ( 25.99999999999999645, 68.00000000000000000, 40.00000000000002132 ) ) ;
#9563 = ORIENTED_EDGE ( 'NONE', *, *, #4491, .F. ) ;
#9564 = DIRECTION ( 'NONE',  ( -1.000000000000000000, -0.000000000000000000, -0.000000000000000000 ) ) ;
#9565 = AXIS2_PLACEMENT_3D ( 'NONE', #3558, #3305, #3643 ) ;
#9566 = CARTESIAN_POINT ( 'NONE',  ( -26.00000000000002132, 10.00000000000000000, 40.00000000000000711 ) ) ;
#9567 = ORIENTED_EDGE ( 'NONE', *, *, #12010, .F. ) ;
#9568 = ADVANCED_FACE ( 'NONE', ( #6750 ), #3534, .F. ) ;
#9569 = EDGE_CURVE ( 'NONE', #2054, #1839, #4100, .T. ) ;
#9570 = ORIENTED_EDGE ( 'NONE', *, *, #4464, .F. ) ;
#9571 = CARTESIAN_POINT ( 'NONE',  ( -45.00000000000000000, 493.2350855268092573, -585.2659423243250103 ) ) ;
#9572 = CARTESIAN_POINT ( 'NONE',  ( 40.00000000000000711, 0.000000000000000000, -34.99999999999997868 ) ) ;
#9573 = ORIENTED_EDGE ( 'NONE', *, *, #2763, .F. ) ;
#9574 = VERTEX_POINT ( 'NONE', #14007 ) ;
#9575 = DIRECTION ( 'NONE',  ( -0.000000000000000000, -0.000000000000000000, 1.000000000000000000 ) ) ;
#9576 = VECTOR ( 'NONE', #9631, 1000.000000000000000 ) ;
#9577 = VERTEX_POINT ( 'NONE', #16663 ) ;
#9578 = ORIENTED_EDGE ( 'NONE', *, *, #6533, .F. ) ;
#9579 = CARTESIAN_POINT ( 'NONE',  ( 10.00000000000000000, -156.2292101480469739, -357.0417483806770633 ) ) ;
#9580 = DIRECTION ( 'NONE',  ( 0.000000000000000000, 0.000000000000000000, 1.000000000000000000 ) ) ;
#9581 = CARTESIAN_POINT ( 'NONE',  ( -150.0000000000000000, 512.1906115401388888, 0.000000000000000000 ) ) ;
#9582 = EDGE_CURVE ( 'NONE', #2950, #13599, #16744, .T. ) ;
#9583 = CARTESIAN_POINT ( 'NONE',  ( 37.00000000000003553, 0.000000000000000000, 20.00000000000000000 ) ) ;
#9584 = DIRECTION ( 'NONE',  ( -0.000000000000000000, -1.000000000000000000, -0.000000000000000000 ) ) ;
#9585 = DIRECTION ( 'NONE',  ( 0.000000000000000000, 1.000000000000000000, -0.000000000000000000 ) ) ;
#9586 = DIRECTION ( 'NONE',  ( 0.000000000000000000, 0.000000000000000000, -1.000000000000000000 ) ) ;
#9587 = CARTESIAN_POINT ( 'NONE',  ( 45.00000000000000000, 549.5810598491749488, -561.6352214130889706 ) ) ;
#9588 = DIRECTION ( 'NONE',  ( -0.000000000000000000, -0.000000000000000000, 1.000000000000000000 ) ) ;
#9589 = ADVANCED_FACE ( 'NONE', ( #2228 ), #10176, .T. ) ;
#9590 = FACE_OUTER_BOUND ( 'NONE', #11835, .T. ) ;
#9591 = LINE ( 'NONE', #8644, #6017 ) ;
#9593 = VERTEX_POINT ( 'NONE', #11428 ) ;
#9592 = EDGE_LOOP ( 'NONE', ( #1822, #8273, #4635, #14295 ) ) ;
#9594 = LINE ( 'NONE', #12336, #5071 ) ;
#9595 = VECTOR ( 'NONE', #9539, 1000.000000000000000 ) ;
#9596 = CARTESIAN_POINT ( 'NONE',  ( 0.3656342590590464514, 286.1036626325263796, 37.32816098065131882 ) ) ;
#9597 = DIRECTION ( 'NONE',  ( 0.000000000000000000, 0.000000000000000000, -1.000000000000000000 ) ) ;
#9598 = FACE_OUTER_BOUND ( 'NONE', #3624, .T. ) ;
#9599 = ORIENTED_EDGE ( 'NONE', *, *, #16223, .T. ) ;
#9600 = EDGE_CURVE ( 'NONE', #4853, #15712, #4896, .T. ) ;
#9601 = EDGE_CURVE ( 'NONE', #16504, #13507, #7779, .T. ) ;
#9602 = FACE_OUTER_BOUND ( 'NONE', #11461, .T. ) ;
#9603 = CIRCLE ( 'NONE', #4651, 29.99999999999530687 ) ;
#9604 = DIRECTION ( 'NONE',  ( 0.000000000000000000, -0.000000000000000000, 1.000000000000000000 ) ) ;
#9605 = ORIENTED_EDGE ( 'NONE', *, *, #12603, .F. ) ;
#9606 = DIRECTION ( 'NONE',  ( 0.000000000000000000, 0.000000000000000000, -1.000000000000000000 ) ) ;
#9607 = AXIS2_PLACEMENT_3D ( 'NONE', #762, #12348, #588 ) ;
#9608 = EDGE_CURVE ( 'NONE', #11869, #2250, #14011, .T. ) ;
#9609 = DIRECTION ( 'NONE',  ( -1.000000000000000000, 0.000000000000000000, 0.000000000000000000 ) ) ;
#9610 = CARTESIAN_POINT ( 'NONE',  ( 6.299999999999999822, -18.50000000000000000, -2.265596578422603396E-15 ) ) ;
#9611 = EDGE_CURVE ( 'NONE', #11869, #9122, #4680, .T. ) ;
#9612 = EDGE_CURVE ( 'NONE', #15922, #6345, #1610, .T. ) ;
#9613 = DIRECTION ( 'NONE',  ( -0.000000000000000000, -0.000000000000000000, 1.000000000000000000 ) ) ;
#9614 = FILL_AREA_STYLE ('',( #10814 ) ) ;
#9615 = CARTESIAN_POINT ( 'NONE',  ( 415.0210210471910841, 329.6061121441327941, 0.000000000000000000 ) ) ;
#9616 = VERTEX_POINT ( 'NONE', #14673 ) ;
#9617 = CARTESIAN_POINT ( 'NONE',  ( 7.000000000000000000, 0.000000000000000000, 0.000000000000000000 ) ) ;
#9618 = AXIS2_PLACEMENT_3D ( 'NONE', #2957, #13270, #1667 ) ;
#9619 = DIRECTION ( 'NONE',  ( -0.000000000000000000, 1.000000000000000000, -0.000000000000000000 ) ) ;
#9620 = AXIS2_PLACEMENT_3D ( 'NONE', #9861, #10030, #510 ) ;
#9621 = DIRECTION ( 'NONE',  ( 0.000000000000000000, 0.000000000000000000, -1.000000000000000000 ) ) ;
#9622 = EDGE_LOOP ( 'NONE', ( #7311, #16849, #16839, #7786 ) ) ;
#9623 = EDGE_CURVE ( 'NONE', #6268, #1132, #14566, .T. ) ;
#9624 = DIRECTION ( 'NONE',  ( 0.000000000000000000, -0.3746065934159096833, 0.9271838545667884235 ) ) ;
#9625 = PRODUCT ( 'Part5', 'Part5', '', ( #790 ) ) ;
#9626 = UNCERTAINTY_MEASURE_WITH_UNIT (LENGTH_MEASURE( 1.000000000000000082E-05 ), #9724, 'distance_accuracy_value', 'NONE');
#9627 = DIRECTION ( 'NONE',  ( -1.803905316987902281E-16, 1.000000000000000000, 0.000000000000000000 ) ) ;
#9628 = ORIENTED_EDGE ( 'NONE', *, *, #14006, .F. ) ;
#9629 = CARTESIAN_POINT ( 'NONE',  ( -10.00000000000000000, 0.000000000000000000, 0.000000000000000000 ) ) ;
#9630 = EDGE_CURVE ( 'NONE', #976, #16546, #580, .T. ) ;
#9631 = DIRECTION ( 'NONE',  ( -1.000000000000000000, -0.000000000000000000, -0.000000000000000000 ) ) ;
#9632 = DIRECTION ( 'NONE',  ( 0.000000000000000000, 0.000000000000000000, 1.000000000000000000 ) ) ;
#9633 = VERTEX_POINT ( 'NONE', #6828 ) ;
#9634 = EDGE_CURVE ( 'NONE', #15340, #9650, #7687, .T. ) ;
#9635 = VECTOR ( 'NONE', #11824, 1000.000000000000000 ) ;
#9636 = EDGE_CURVE ( 'NONE', #11171, #12242, #2901, .T. ) ;
#9637 = ADVANCED_FACE ( 'NONE', ( #327 ), #7086, .T. ) ;
#9638 = PRESENTATION_STYLE_ASSIGNMENT (( #8339 ) ) ;
#9639 = ORIENTED_EDGE ( 'NONE', *, *, #14392, .F. ) ;
#9640 =( REPRESENTATION_RELATIONSHIP ('NONE','NONE', #15277, #584 ) REPRESENTATION_RELATIONSHIP_WITH_TRANSFORMATION ( #3954 )SHAPE_REPRESENTATION_RELATIONSHIP( ) );
#9641 = ORIENTED_EDGE ( 'NONE', *, *, #6851, .T. ) ;
#9642 = PLANE ( 'NONE',  #16584 ) ;
#9643 = ORIENTED_EDGE ( 'NONE', *, *, #9488, .T. ) ;
#9644 = APPLICATION_PROTOCOL_DEFINITION ( 'draft international standard', 'automotive_design', 1998, #4675 ) ;
#9645 = ORIENTED_EDGE ( 'NONE', *, *, #14679, .T. ) ;
#9646 = CIRCLE ( 'NONE', #2220, 15.25000000000000000 ) ;
#9647 = VERTEX_POINT ( 'NONE', #8479 ) ;
#9648 = CARTESIAN_POINT ( 'NONE',  ( 1.347066989204613998E-15, 0.000000000000000000, 22.00000000000000000 ) ) ;
#9649 = LINE ( 'NONE', #5768, #9730 ) ;
#9650 = VERTEX_POINT ( 'NONE', #15941 ) ;
#9651 = DIRECTION ( 'NONE',  ( 0.000000000000000000, 0.000000000000000000, 1.000000000000000000 ) ) ;
#9652 = DIRECTION ( 'NONE',  ( 0.000000000000000000, 0.000000000000000000, -1.000000000000000000 ) ) ;
#9653 = EDGE_LOOP ( 'NONE', ( #7373, #3248, #13172, #12807 ) ) ;
#9654 = ADVANCED_FACE ( 'NONE', ( #666 ), #500, .T. ) ;
#9655 = FILL_AREA_STYLE ('',( #10594 ) ) ;
#9656 = VERTEX_POINT ( 'NONE', #4282 ) ;
#9657 = DIRECTION ( 'NONE',  ( -1.000000000000000000, -0.000000000000000000, -0.000000000000000000 ) ) ;
#9658 = DIRECTION ( 'NONE',  ( -1.000000000000000000, -0.000000000000000000, -0.000000000000000000 ) ) ;
#9659 = ORIENTED_EDGE ( 'NONE', *, *, #264, .T. ) ;
#9660 = TOROIDAL_SURFACE ( 'NONE', #5804, 4.695405383895982609, 9.000000000000000000 ) ;
#9661 = VERTEX_POINT ( 'NONE', #2981 ) ;
#9662 = CARTESIAN_POINT ( 'NONE',  ( 30.90550859392665473, -37.11391548236653648, 66.87703344121199223 ) ) ;
#9663 = CARTESIAN_POINT ( 'NONE',  ( -2.216159785453297477E-13, 104.2500000000000142, 0.000000000000000000 ) ) ;
#9664 = AXIS2_PLACEMENT_3D ( 'NONE', #15578, #6367, #987 ) ;
#9665 = AXIS2_PLACEMENT_3D ( 'NONE', #15867, #12275, #8411 ) ;
#9666 = CIRCLE ( 'NONE', #3343, 187.4999999999998863 ) ;
#9667 = EDGE_LOOP ( 'NONE', ( #11214, #6340 ) ) ;
#9668 = ORIENTED_EDGE ( 'NONE', *, *, #10607, .F. ) ;
#9669 = CARTESIAN_POINT ( 'NONE',  ( -0.7824566857511718876, 38.09717326031902473, 9.469691317190788382 ) ) ;
#9670 = EDGE_CURVE ( 'NONE', #10121, #3447, #7411, .T. ) ;
#9671 = PLANE ( 'NONE',  #3338 ) ;
#9672 = CARTESIAN_POINT ( 'NONE',  ( -34.99999999999999289, 0.000000000000000000, -35.00000000000000711 ) ) ;
#9673 = CIRCLE ( 'NONE', #3907, 0.7366000000000039183 ) ;
#9674 = LINE ( 'NONE', #14904, #12298 ) ;
#9675 = CYLINDRICAL_SURFACE ( 'NONE', #8328, 18.50000000000000000 ) ;
#9676 = ADVANCED_FACE ( 'NONE', ( #12179 ), #5805, .F. ) ;
#9677 = FACE_OUTER_BOUND ( 'NONE', #3979, .T. ) ;
#9678 = AXIS2_PLACEMENT_3D ( 'NONE', #1170, #16879, #7767 ) ;
#9679 = CARTESIAN_POINT ( 'NONE',  ( -55.99999999999988631, 645.2345343053611941, -411.3640676610526157 ) ) ;
#9680 = VECTOR ( 'NONE', #13623, 1000.000000000000000 ) ;
#9681 = CARTESIAN_POINT ( 'NONE',  ( 65.00000000000000000, 380.0000000000000000, -7.000000000000006217 ) ) ;
#9682 = CARTESIAN_POINT ( 'NONE',  ( 40.00000000000000711, 19.00000000000000000, 25.99999999999999645 ) ) ;
#9683 = DIRECTION ( 'NONE',  ( -1.000000000000000000, -0.000000000000000000, -0.000000000000000000 ) ) ;
#9684 = LINE ( 'NONE', #1604, #4399 ) ;
#9686 = VERTEX_POINT ( 'NONE', #13717 ) ;
#9685 = ORIENTED_EDGE ( 'NONE', *, *, #7304, .T. ) ;
#9687 = AXIS2_PLACEMENT_3D ( 'NONE', #2553, #8926, #14164 ) ;
#9688 = CARTESIAN_POINT ( 'NONE',  ( 0.000000000000000000, 50.00000000000000000, 0.000000000000000000 ) ) ;
#9689 = PRODUCT_DEFINITION ( 'UNKNOWN', '', #4238, #3096 ) ;
#9690 = DIRECTION ( 'NONE',  ( -0.000000000000000000, -1.000000000000000000, -0.000000000000000000 ) ) ;
#9691 = VECTOR ( 'NONE', #2648, 1000.000000000000000 ) ;
#9692 = CARTESIAN_POINT ( 'NONE',  ( 27.49999999999999645, 196.3050121726289206, -17.00000000000000000 ) ) ;
#9693 = CARTESIAN_POINT ( 'NONE',  ( 10.00000000000000000, 381.0487089519826895, 2.719601036885452502E-12 ) ) ;
#9694 = ORIENTED_EDGE ( 'NONE', *, *, #4662, .F. ) ;
#9695 = AXIS2_PLACEMENT_3D ( 'NONE', #16253, #5426, #3035 ) ;
#9696 = DIRECTION ( 'NONE',  ( -0.000000000000000000, -1.000000000000000000, -0.000000000000000000 ) ) ;
#9697 = ORIENTED_EDGE ( 'NONE', *, *, #13215, .T. ) ;
#9698 = DIRECTION ( 'NONE',  ( -1.000000000000000000, 0.000000000000000000, 0.000000000000000000 ) ) ;
#9699 = CARTESIAN_POINT ( 'NONE',  ( -2.493494276495503037, 191.0031835148159303, 37.61078711647776629 ) ) ;
#9700 = LINE ( 'NONE', #1701, #12387 ) ;
#9701 = AXIS2_PLACEMENT_3D ( 'NONE', #10136, #863, #7452 ) ;
#9702 = DIRECTION ( 'NONE',  ( 0.000000000000000000, 0.000000000000000000, 1.000000000000000000 ) ) ;
#9703 = AXIS2_PLACEMENT_3D ( 'NONE', #244, #5729, #1438 ) ;
#9704 = FACE_OUTER_BOUND ( 'NONE', #7694, .T. ) ;
#9705 = VERTEX_POINT ( 'NONE', #10968 ) ;
#9706 = DIRECTION ( 'NONE',  ( 0.000000000000000000, 0.000000000000000000, -1.000000000000000000 ) ) ;
#9707 = EDGE_CURVE ( 'NONE', #5261, #8106, #1390, .T. ) ;
#9708 = AXIS2_PLACEMENT_3D ( 'NONE', #1215, #1045, #4978 ) ;
#9709 = LINE ( 'NONE', #1550, #16710 ) ;
#9710 = CARTESIAN_POINT ( 'NONE',  ( -21.00000000000002842, 0.000000000000000000, -34.99999999999999289 ) ) ;
#9711 = CONICAL_SURFACE ( 'NONE', #15461, 0.9999999999999950040, 1.029744258676644320 ) ;
#9712 = ADVANCED_FACE ( 'NONE', ( #13471 ), #13385, .F. ) ;
#9713 = ORIENTED_EDGE ( 'NONE', *, *, #2061, .F. ) ;
#9714 = AXIS2_PLACEMENT_3D ( 'NONE', #15762, #13192, #15596 ) ;
#9715 = AXIS2_PLACEMENT_3D ( 'NONE', #10951, #4426, #3387 ) ;
#9716 = FACE_BOUND ( 'NONE', #12918, .T. ) ;
#9717 = CYLINDRICAL_SURFACE ( 'NONE', #7291, 3.300000000000011369 ) ;
#9718 = ORIENTED_EDGE ( 'NONE', *, *, #700, .F. ) ;
#9719 = DIRECTION ( 'NONE',  ( -0.000000000000000000, -1.000000000000000000, -0.000000000000000000 ) ) ;
#9720 = VECTOR ( 'NONE', #2629, 1000.000000000000000 ) ;
#9721 = LINE ( 'NONE', #11242, #4358 ) ;
#9722 = CARTESIAN_POINT ( 'NONE',  ( -32.00000000000000711, 10.00000000000000000, -22.00000000000000355 ) ) ;
#9723 = EDGE_LOOP ( 'NONE', ( #16261, #805, #5011, #11231, #6703 ) ) ;
#9724 =( LENGTH_UNIT ( ) NAMED_UNIT ( * ) SI_UNIT ( .MILLI., .METRE. ) );
#9725 = VERTEX_POINT ( 'NONE', #9692 ) ;
#9726 = ORIENTED_EDGE ( 'NONE', *, *, #1301, .F. ) ;
#9727 = CIRCLE ( 'NONE', #4507, 3.000000000000002665 ) ;
#9728 = DIRECTION ( 'NONE',  ( 1.000000000000000000, 0.000000000000000000, 0.000000000000000000 ) ) ;
#9729 = EDGE_CURVE ( 'NONE', #15829, #5489, #5643, .T. ) ;
#9730 = VECTOR ( 'NONE', #715, 1000.000000000000000 ) ;
#9731 = ORIENTED_EDGE ( 'NONE', *, *, #8774, .T. ) ;
#9732 = APPLICATION_PROTOCOL_DEFINITION ( 'draft international standard', 'automotive_design', 1998, #6196 ) ;
#9733 = CIRCLE ( 'NONE', #7505, 22.75209553982837463 ) ;
#9734 = ORIENTED_EDGE ( 'NONE', *, *, #3318, .T. ) ;
#9735 = ADVANCED_FACE ( 'NONE', ( #4188 ), #14838, .F. ) ;
#9736 = DIRECTION ( 'NONE',  ( 0.000000000000000000, 0.000000000000000000, -1.000000000000000000 ) ) ;
#9737 = EDGE_CURVE ( 'NONE', #13073, #155, #11269, .T. ) ;
#9738 = EDGE_CURVE ( 'NONE', #6153, #12411, #6043, .T. ) ;
#9739 = EDGE_LOOP ( 'NONE', ( #2781, #14620, #11067, #10578 ) ) ;
#9740 = EDGE_CURVE ( 'NONE', #414, #7123, #6216, .T. ) ;
#9741 = DIRECTION ( 'NONE',  ( 0.000000000000000000, 0.000000000000000000, -1.000000000000000000 ) ) ;
#9742 = DIRECTION ( 'NONE',  ( -1.000000000000000000, -0.000000000000000000, 0.000000000000000000 ) ) ;
#9743 = ORIENTED_EDGE ( 'NONE', *, *, #600, .T. ) ;
#9744 = DIRECTION ( 'NONE',  ( -0.000000000000000000, -1.000000000000000000, -0.000000000000000000 ) ) ;
#9745 = AXIS2_PLACEMENT_3D ( 'NONE', #4610, #10106, #4861 ) ;
#9746 = APPLICATION_CONTEXT ( 'automotive_design' ) ;
#9747 = CARTESIAN_POINT ( 'NONE',  ( 6.237780304489215888E-13, 189.4632308570089094, 37.52989836422088388 ) ) ;
#9748 = ORIENTED_EDGE ( 'NONE', *, *, #10244, .T. ) ;
#9749 = CIRCLE ( 'NONE', #2319, 0.7365999999987737912 ) ;
#9750 =( NAMED_UNIT ( * ) SI_UNIT ( $, .STERADIAN. ) SOLID_ANGLE_UNIT ( ) );
#9751 = ORIENTED_EDGE ( 'NONE', *, *, #10628, .F. ) ;
#9752 = DIRECTION ( 'NONE',  ( -1.000000000000000000, 0.000000000000000000, 0.000000000000000000 ) ) ;
#9753 = ORIENTED_EDGE ( 'NONE', *, *, #7282, .F. ) ;
#9754 = ORIENTED_EDGE ( 'NONE', *, *, #1200, .F. ) ;
#9755 = PLANE ( 'NONE',  #10775 ) ;
#9756 = ORIENTED_EDGE ( 'NONE', *, *, #6395, .T. ) ;
#9757 = ORIENTED_EDGE ( 'NONE', *, *, #15377, .T. ) ;
#9758 = CARTESIAN_POINT ( 'NONE',  ( -10.00000000000000000, 0.000000000000000000, 22.49999999999999645 ) ) ;
#9759 = VECTOR ( 'NONE', #8555, 1000.000000000000000 ) ;
#9760 = ADVANCED_FACE ( 'NONE', ( #8735, #4856 ), #13883, .T. ) ;
#9761 = LINE ( 'NONE', #562, #15939 ) ;
#9762 = DIRECTION ( 'NONE',  ( -0.4740998230350218501, -0.8804710999221728729, -1.078266114261438272E-16 ) ) ;
#9763 = DIRECTION ( 'NONE',  ( 0.000000000000000000, 0.000000000000000000, 1.000000000000000000 ) ) ;
#9764 = PRODUCT_DEFINITION_SHAPE ( 'NONE', 'NONE',  #16968 ) ;
#9765 = CARTESIAN_POINT ( 'NONE',  ( -18.00000000000000711, 0.000000000000000000, 0.000000000000000000 ) ) ;
#9766 = DIRECTION ( 'NONE',  ( -1.000000000000000000, -0.000000000000000000, -0.000000000000000000 ) ) ;
#9767 = DIRECTION ( 'NONE',  ( 1.000000000000000000, 0.000000000000000000, 0.000000000000000000 ) ) ;
#9768 = VERTEX_POINT ( 'NONE', #2109 ) ;
#9769 = CARTESIAN_POINT ( 'NONE',  ( -46.99999999999988631, 549.5810598491749488, -570.6352214130889706 ) ) ;
#9770 = DIRECTION ( 'NONE',  ( 0.000000000000000000, 0.000000000000000000, 1.000000000000000000 ) ) ;
#9771 = VECTOR ( 'NONE', #1408, 1000.000000000000000 ) ;
#9772 = CARTESIAN_POINT ( 'NONE',  ( 394.0000000000001137, 240.7889724647196488, -17.15546574335979813 ) ) ;
#9773 = DIRECTION ( 'NONE',  ( 1.000000000000000000, 0.000000000000000000, 0.000000000000000000 ) ) ;
#9775 = ORIENTED_EDGE ( 'NONE', *, *, #8155, .F. ) ;
#9774 = ORIENTED_EDGE ( 'NONE', *, *, #14747, .F. ) ;
#9776 = CARTESIAN_POINT ( 'NONE',  ( 3.000000000000000000, 6.000000000000000000, 3.000000000000000000 ) ) ;
#9777 = CYLINDRICAL_SURFACE ( 'NONE', #3886, 13.69540538389601991 ) ;
#9778 = DIRECTION ( 'NONE',  ( 1.000000000000000000, -0.000000000000000000, -0.000000000000000000 ) ) ;
#9779 = CARTESIAN_POINT ( 'NONE',  ( 5.569974746830579804, 0.000000000000000000, -14.76997474683060041 ) ) ;
#9780 = TOROIDAL_SURFACE ( 'NONE', #8943, 22.46376988133006236, 4.000164074322307250 ) ;
#9781 = ORIENTED_EDGE ( 'NONE', *, *, #6080, .T. ) ;
#9782 = AXIS2_PLACEMENT_3D ( 'NONE', #14474, #10685, #14642 ) ;
#9783 = DIRECTION ( 'NONE',  ( 0.000000000000000000, 1.000000000000000000, 0.000000000000000000 ) ) ;
#9784 = ORIENTED_EDGE ( 'NONE', *, *, #10985, .T. ) ;
#9785 = LINE ( 'NONE', #14304, #10699 ) ;
#9786 = CARTESIAN_POINT ( 'NONE',  ( 0.5437965083814821909, 192.7427235764099578, 37.26905881172010737 ) ) ;
#9787 = CARTESIAN_POINT ( 'NONE',  ( -10.00000000000000000, 2.755455298081544383E-15, -22.49999999999999645 ) ) ;
#9788 = DIRECTION ( 'NONE',  ( 0.000000000000000000, 0.000000000000000000, 1.000000000000000000 ) ) ;
#9789 = LINE ( 'NONE', #4543, #12009 ) ;
#9790 = ORIENTED_EDGE ( 'NONE', *, *, #2090, .F. ) ;
#9791 = VECTOR ( 'NONE', #10112, 1000.000000000000000 ) ;
#9792 = CARTESIAN_POINT ( 'NONE',  ( 10.00000000000000000, 202.9739201934855828, -514.2167050642598269 ) ) ;
#9793 = CIRCLE ( 'NONE', #10053, 84.99999999999997158 ) ;
#9794 = DIRECTION ( 'NONE',  ( -1.000000000000000000, -0.000000000000000000, 0.000000000000000000 ) ) ;
#9795 = DIRECTION ( 'NONE',  ( -1.000000000000000000, 0.000000000000000000, -3.854941057726246479E-16 ) ) ;
#9796 = ORIENTED_EDGE ( 'NONE', *, *, #16445, .T. ) ;
#9797 = DIRECTION ( 'NONE',  ( 0.000000000000000000, -0.000000000000000000, -1.000000000000000000 ) ) ;
#9798 = CIRCLE ( 'NONE', #9531, 4.999999999999997335 ) ;
#9799 = ADVANCED_FACE ( 'NONE', ( #755 ), #16377, .T. ) ;
#9800 = CARTESIAN_POINT ( 'NONE',  ( 10.00000000000000000, 435.2933666400819561, -550.3792044179907634 ) ) ;
#9801 = ORIENTED_EDGE ( 'NONE', *, *, #10766, .T. ) ;
#9802 = VECTOR ( 'NONE', #2907, 1000.000000000000000 ) ;
#9803 = CARTESIAN_POINT ( 'NONE',  ( 26.00000000000000711, 68.00000000000000000, -31.00000000000002487 ) ) ;
#9804 = EDGE_CURVE ( 'NONE', #14998, #1375, #10184, .T. ) ;
#9805 = DIRECTION ( 'NONE',  ( 0.000000000000000000, 0.000000000000000000, 1.000000000000000000 ) ) ;
#9806 = CARTESIAN_POINT ( 'NONE',  ( 1.750000000000000000, 0.000000000000000000, 0.000000000000000000 ) ) ;
#9807 = EDGE_LOOP ( 'NONE', ( #7021, #532, #16728, #12041 ) ) ;
#9808 = FILL_AREA_STYLE ('',( #1893 ) ) ;
#9809 = VERTEX_POINT ( 'NONE', #12844 ) ;
#9810 = ORIENTED_EDGE ( 'NONE', *, *, #16955, .F. ) ;
#9811 = EDGE_CURVE ( 'NONE', #3550, #5229, #16453, .T. ) ;
#9812 = CARTESIAN_POINT ( 'NONE',  ( -440.0000000000000568, 620.7506394335853201, -11.00000000000000000 ) ) ;
#9813 = CONTEXT_DEPENDENT_SHAPE_REPRESENTATION ( #954, #14823 ) ;
#9814 = CARTESIAN_POINT ( 'NONE',  ( 2.694300560877697759, 61.33377131228787249, 9.110264267939502503 ) ) ;
#9815 = VERTEX_POINT ( 'NONE', #8811 ) ;
#9816 = DIRECTION ( 'NONE',  ( 0.000000000000000000, 0.000000000000000000, -1.000000000000000000 ) ) ;
#9817 = CARTESIAN_POINT ( 'NONE',  ( 0.000000000000000000, 10.00000000000000000, 0.000000000000000000 ) ) ;
#9818 = ADVANCED_FACE ( 'NONE', ( #15257 ), #8906, .T. ) ;
#9819 = VERTEX_POINT ( 'NONE', #6135 ) ;
#9820 = LINE ( 'NONE', #15046, #11345 ) ;
#9821 = CARTESIAN_POINT ( 'NONE',  ( 0.000000000000000000, 202.9739201934855828, -514.2167050642598269 ) ) ;
#9822 = ORIENTED_EDGE ( 'NONE', *, *, #10235, .F. ) ;
#9823 = SURFACE_STYLE_FILL_AREA ( #3463 ) ;
#9824 = ADVANCED_FACE ( 'NONE', ( #15419 ), #7256, .F. ) ;
#9825 = EDGE_LOOP ( 'NONE', ( #9743, #9378, #11741, #6171 ) ) ;
#9826 = VERTEX_POINT ( 'NONE', #3664 ) ;
#9827 = EDGE_CURVE ( 'NONE', #377, #14070, #12764, .T. ) ;
#9828 = EDGE_CURVE ( 'NONE', #14719, #4224, #10022, .T. ) ;
#9829 = EDGE_LOOP ( 'NONE', ( #5563, #5581 ) ) ;
#9830 =( NAMED_UNIT ( * ) PLANE_ANGLE_UNIT ( ) SI_UNIT ( $, .RADIAN. ) );
#9831 = ORIENTED_EDGE ( 'NONE', *, *, #6866, .T. ) ;
#9832 = VERTEX_POINT ( 'NONE', #2025 ) ;
#9833 = CARTESIAN_POINT ( 'NONE',  ( -55.99999999999989342, 493.2350855268086320, -494.4847040861889127 ) ) ;
#9834 = AXIS2_PLACEMENT_3D ( 'NONE', #4916, #8883, #12575 ) ;
#9835 = DIRECTION ( 'NONE',  ( -1.000000000000000000, 0.000000000000000000, -0.000000000000000000 ) ) ;
#9836 = DIRECTION ( 'NONE',  ( -1.000000000000000000, 0.000000000000000000, -0.000000000000000000 ) ) ;
#9837 = CARTESIAN_POINT ( 'NONE',  ( -34.99999999999999289, 11.00000000000000000, 40.00000000000000711 ) ) ;
#9838 = DIRECTION ( 'NONE',  ( -1.000000000000000000, 0.000000000000000000, -0.000000000000000000 ) ) ;
#9839 = DIRECTION ( 'NONE',  ( -1.000000000000000000, 0.000000000000000000, -1.631319816340925608E-17 ) ) ;
#9840 = CARTESIAN_POINT ( 'NONE',  ( -33.00000000000000000, 8.000000000000000000, -26.00000000000000355 ) ) ;
#9841 = ADVANCED_FACE ( 'NONE', ( #13967 ), #16623, .F. ) ;
#9842 = ORIENTED_EDGE ( 'NONE', *, *, #13099, .F. ) ;
#9843 = DIRECTION ( 'NONE',  ( 0.000000000000000000, 0.000000000000000000, -1.000000000000000000 ) ) ;
#9844 = DIRECTION ( 'NONE',  ( 1.000000000000000000, 0.000000000000000000, 0.000000000000000000 ) ) ;
#9845 = EDGE_CURVE ( 'NONE', #11441, #4991, #10438, .T. ) ;
#9846 = EDGE_CURVE ( 'NONE', #1132, #8130, #11137, .T. ) ;
#9847 = CARTESIAN_POINT ( 'NONE',  ( -10.00000000000000000, 0.000000000000000000, 0.000000000000000000 ) ) ;
#9848 = VECTOR ( 'NONE', #3691, 1000.000000000000000 ) ;
#9849 = CARTESIAN_POINT ( 'NONE',  ( 10.00000000000000000, 364.9870314427736275, -216.3519347178565795 ) ) ;
#9851 = EDGE_LOOP ( 'NONE', ( #8295, #15371, #8611, #3980 ) ) ;
#9850 = ORIENTED_EDGE ( 'NONE', *, *, #9804, .F. ) ;
#9852 = DIRECTION ( 'NONE',  ( 1.000000000000000000, 0.000000000000000000, 0.000000000000000000 ) ) ;
#9853 = ORIENTED_EDGE ( 'NONE', *, *, #11101, .T. ) ;
#9854 = CARTESIAN_POINT ( 'NONE',  ( 5.941205806953520074, -15.14120580695428764, -1.854262922671788806E-15 ) ) ;
#9855 = DIRECTION ( 'NONE',  ( 1.000000000000000000, -0.000000000000000000, -0.000000000000000000 ) ) ;
#9856 = EDGE_LOOP ( 'NONE', ( #5703, #12562 ) ) ;
#9857 = FACE_OUTER_BOUND ( 'NONE', #8808, .T. ) ;
#9858 =( REPRESENTATION_RELATIONSHIP ('NONE','NONE', #15822, #7583 ) REPRESENTATION_RELATIONSHIP_WITH_TRANSFORMATION ( #7085 )SHAPE_REPRESENTATION_RELATIONSHIP( ) );
#9859 = CARTESIAN_POINT ( 'NONE',  ( -8.881784197001250351E-16, 0.000000000000000000, 0.000000000000000000 ) ) ;
#9860 = ORIENTED_EDGE ( 'NONE', *, *, #8958, .F. ) ;
#9861 = CARTESIAN_POINT ( 'NONE',  ( 31.00000000000001421, 10.00000000000000000, 22.99999999999999645 ) ) ;
#9862 = CARTESIAN_POINT ( 'NONE',  ( 0.7366000000000042514, 192.7498655622790977, 37.20123489369387926 ) ) ;
#9863 = PLANE ( 'NONE',  #8288 ) ;
#9864 = VECTOR ( 'NONE', #14399, 1000.000000000000000 ) ;
#9865 = PLANE ( 'NONE',  #3436 ) ;
#9866 = DIRECTION ( 'NONE',  ( -0.000000000000000000, -1.000000000000000000, -0.000000000000000000 ) ) ;
#9867 = ORIENTED_EDGE ( 'NONE', *, *, #11193, .F. ) ;
#9868 = CARTESIAN_POINT ( 'NONE',  ( 10.00000000000000000, 435.2933666400819561, -550.3792044179907634 ) ) ;
#9869 = LINE ( 'NONE', #1881, #16168 ) ;
#9870 = ORIENTED_EDGE ( 'NONE', *, *, #5097, .T. ) ;
#9871 = PLANE ( 'NONE',  #13528 ) ;
#9872 = VECTOR ( 'NONE', #13984, 1000.000000000000000 ) ;
#9873 = ORIENTED_EDGE ( 'NONE', *, *, #12459, .F. ) ;
#9874 = DIRECTION ( 'NONE',  ( 0.000000000000000000, 1.000000000000000000, 0.000000000000000000 ) ) ;
#9875 = EDGE_CURVE ( 'NONE', #9087, #16075, #5216, .T. ) ;
#9876 = DIRECTION ( 'NONE',  ( -0.000000000000000000, 0.000000000000000000, 1.000000000000000000 ) ) ;
#9877 = ORIENTED_EDGE ( 'NONE', *, *, #14865, .T. ) ;
#9878 = CARTESIAN_POINT ( 'NONE',  ( 20.99999999999996092, -20.00000000000000000, 32.50000000000000711 ) ) ;
#9879 = DIRECTION ( 'NONE',  ( 0.000000000000000000, 0.000000000000000000, -1.000000000000000000 ) ) ;
#9880 = CARTESIAN_POINT ( 'NONE',  ( -25.99999999999999645, 68.00000000000000000, 40.00000000000002132 ) ) ;
#9881 = ORIENTED_EDGE ( 'NONE', *, *, #806, .T. ) ;
#9882 = EDGE_CURVE ( 'NONE', #7408, #15471, #9093, .T. ) ;
#9883 = DIRECTION ( 'NONE',  ( 0.000000000000000000, 0.000000000000000000, -1.000000000000000000 ) ) ;
#9884 = VERTEX_POINT ( 'NONE', #9854 ) ;
#9885 = ORIENTED_EDGE ( 'NONE', *, *, #6250, .F. ) ;
#9886 = AXIS2_PLACEMENT_3D ( 'NONE', #5543, #7004, #10793 ) ;
#9887 = DIRECTION ( 'NONE',  ( 0.000000000000000000, 0.000000000000000000, 1.000000000000000000 ) ) ;
#9888 = VECTOR ( 'NONE', #6926, 1000.000000000000000 ) ;
#9889 = APPLICATION_PROTOCOL_DEFINITION ( 'draft international standard', 'automotive_design', 1998, #8850 ) ;
#9890 = PRODUCT_RELATED_PRODUCT_CATEGORY ( 'part', '', ( #1513 ) ) ;
#9891 = DIRECTION ( 'NONE',  ( 0.000000000000000000, 0.000000000000000000, -1.000000000000000000 ) ) ;
#9892 = ORIENTED_EDGE ( 'NONE', *, *, #14433, .T. ) ;
#9893 = LINE ( 'NONE', #4568, #9377 ) ;
#9894 = PLANE ( 'NONE',  #3418 ) ;
#9895 = ADVANCED_FACE ( 'NONE', ( #8563 ), #14561, .T. ) ;
#9896 = VECTOR ( 'NONE', #2583, 1000.000000000000000 ) ;
#9897 = ORIENTED_EDGE ( 'NONE', *, *, #1858, .F. ) ;
#9898 = DIRECTION ( 'NONE',  ( -0.000000000000000000, -1.000000000000000000, -0.000000000000000000 ) ) ;
#9899 = CARTESIAN_POINT ( 'NONE',  ( -3.270000000000000462, 284.6994879831845537, 28.46994879831456515 ) ) ;
#9900 = VERTEX_POINT ( 'NONE', #6549 ) ;
#9901 = DIRECTION ( 'NONE',  ( 0.000000000000000000, 0.000000000000000000, 1.000000000000000000 ) ) ;
#9902 = ORIENTED_EDGE ( 'NONE', *, *, #2080, .T. ) ;
#9903 = ORIENTED_EDGE ( 'NONE', *, *, #3834, .F. ) ;
#9904 = ORIENTED_EDGE ( 'NONE', *, *, #5097, .F. ) ;
#9905 = CIRCLE ( 'NONE', #15384, 13.69540538389601991 ) ;
#9906 = ADVANCED_FACE ( 'NONE', ( #2528 ), #16783, .T. ) ;
#9907 = ORIENTED_EDGE ( 'NONE', *, *, #15589, .T. ) ;
#9908 = EDGE_LOOP ( 'NONE', ( #3608, #16724, #5167, #4143 ) ) ;
#9909 = DIRECTION ( 'NONE',  ( 1.000000000000000000, 0.000000000000000000, -0.000000000000000000 ) ) ;
#9910 = DIRECTION ( 'NONE',  ( 0.000000000000000000, 1.000000000000000000, 1.224646799147353207E-16 ) ) ;
#9911 = DIRECTION ( 'NONE',  ( 1.000000000000000000, 0.000000000000000000, 0.000000000000000000 ) ) ;
#9912 = EDGE_CURVE ( 'NONE', #377, #4587, #8540, .T. ) ;
#9913 = EDGE_CURVE ( 'NONE', #976, #377, #1413, .T. ) ;
#9914 = DIRECTION ( 'NONE',  ( 0.000000000000000000, 0.000000000000000000, -1.000000000000000000 ) ) ;
#9915 = PLANE ( 'NONE',  #89 ) ;
#9916 = DIRECTION ( 'NONE',  ( 0.000000000000000000, 0.000000000000000000, -1.000000000000000000 ) ) ;
#9917 = AXIS2_PLACEMENT_3D ( 'NONE', #6635, #3750, #11897 ) ;
#9918 = LINE ( 'NONE', #7149, #572 ) ;
#9919 = DIRECTION ( 'NONE',  ( 0.000000000000000000, 9.899245676326632924E-17, 1.000000000000000000 ) ) ;
#9920 = VERTEX_POINT ( 'NONE', #2621 ) ;
#9921 = CARTESIAN_POINT ( 'NONE',  ( 26.00000000000000000, 19.00000000000000000, -40.00000000000000711 ) ) ;
#9922 = FACE_OUTER_BOUND ( 'NONE', #14573, .T. ) ;
#9923 = AXIS2_PLACEMENT_3D ( 'NONE', #14848, #4198, #10716 ) ;
#9924 = FACE_OUTER_BOUND ( 'NONE', #4576, .T. ) ;
#9925 = CARTESIAN_POINT ( 'NONE',  ( 0.7365999999999666148, 289.4632308570086252, 37.52989836422090519 ) ) ;
#9927 = ORIENTED_EDGE ( 'NONE', *, *, #4142, .F. ) ;
#9926 = ORIENTED_EDGE ( 'NONE', *, *, #8917, .T. ) ;
#9928 = CARTESIAN_POINT ( 'NONE',  ( 10.00000000000000000, 620.7506394335853201, 0.000000000000000000 ) ) ;
#9929 = EDGE_CURVE ( 'NONE', #14215, #3627, #6065, .T. ) ;
#9930 = VERTEX_POINT ( 'NONE', #5106 ) ;
#9931 = VECTOR ( 'NONE', #11013, 1000.000000000000000 ) ;
#9932 =( NAMED_UNIT ( * ) SI_UNIT ( $, .STERADIAN. ) SOLID_ANGLE_UNIT ( ) );
#9933 = DIRECTION ( 'NONE',  ( -1.000000000000000000, 0.000000000000000000, 0.000000000000000000 ) ) ;
#9934 = EDGE_CURVE ( 'NONE', #3903, #7845, #14576, .T. ) ;
#9935 = CARTESIAN_POINT ( 'NONE',  ( -55.99999999999989342, 559.9933750504617365, -533.0276205133087615 ) ) ;
#9936 = ADVANCED_FACE ( 'NONE', ( #1333 ), #6053, .T. ) ;
#9938 = ORIENTED_EDGE ( 'NONE', *, *, #1417, .F. ) ;
#9937 = EDGE_CURVE ( 'NONE', #11353, #9952, #16949, .T. ) ;
#9939 = AXIS2_PLACEMENT_3D ( 'NONE', #9615, #14851, #12193 ) ;
#9940 = EDGE_CURVE ( 'NONE', #4506, #14978, #6886, .T. ) ;
#9941 = AXIS2_PLACEMENT_3D ( 'NONE', #15268, #4615, #11148 ) ;
#9942 = AXIS2_PLACEMENT_3D ( 'NONE', #11944, #11762, #2482 ) ;
#9943 = DIRECTION ( 'NONE',  ( -0.000000000000000000, 1.000000000000000000, 1.224646799147353207E-16 ) ) ;
#9944 = CARTESIAN_POINT ( 'NONE',  ( -22.00000000000001776, 10.00000000000000000, 33.00000000000000711 ) ) ;
#9945 = ORIENTED_EDGE ( 'NONE', *, *, #3943, .T. ) ;
#9946 = CARTESIAN_POINT ( 'NONE',  ( -1.845421771225094876, 62.39699037330763076, 9.323305159997635982 ) ) ;
#9947 = CARTESIAN_POINT ( 'NONE',  ( 0.2120431089105883071, 189.4665537169271374, 37.56312696337839441 ) ) ;
#9948 = DIRECTION ( 'NONE',  ( -1.000000000000000000, -0.000000000000000000, -0.000000000000000000 ) ) ;
#9949 = VECTOR ( 'NONE', #11764, 1000.000000000000000 ) ;
#9950 = CARTESIAN_POINT ( 'NONE',  ( 415.0210210471910841, 329.6061121441327941, -10.00000000000000000 ) ) ;
#9951 = CARTESIAN_POINT ( 'NONE',  ( -3.000000000000000000, 41.00000000000000711, 6.000000000000000000 ) ) ;
#9952 = VERTEX_POINT ( 'NONE', #10519 ) ;
#9953 = CARTESIAN_POINT ( 'NONE',  ( 175.0000000000000568, 515.4878487013597805, -546.7230258972048205 ) ) ;
#9954 = DIRECTION ( 'NONE',  ( 0.000000000000000000, 0.000000000000000000, 1.000000000000000000 ) ) ;
#9955 = VERTEX_POINT ( 'NONE', #1249 ) ;
#9956 = DIRECTION ( 'NONE',  ( 3.854941057726246479E-16, 0.000000000000000000, -1.000000000000000000 ) ) ;
#9957 = AXIS2_PLACEMENT_3D ( 'NONE', #16043, #5554, #14761 ) ;
#9958 = EDGE_LOOP ( 'NONE', ( #1556, #6615, #9487, #2215 ) ) ;
#9959 = EDGE_CURVE ( 'NONE', #1511, #15922, #15757, .T. ) ;
#9960 = DIRECTION ( 'NONE',  ( 0.000000000000000000, 0.000000000000000000, -1.000000000000000000 ) ) ;
#9961 = LINE ( 'NONE', #12612, #460 ) ;
#9962 = ORIENTED_EDGE ( 'NONE', *, *, #2364, .T. ) ;
#9963 = CYLINDRICAL_SURFACE ( 'NONE', #2580, 5.000000000000000888 ) ;
#9964 = VECTOR ( 'NONE', #4075, 1000.000000000000000 ) ;
#9965 = CIRCLE ( 'NONE', #7472, 4.695405383896011919 ) ;
#9966 = FACE_OUTER_BOUND ( 'NONE', #15442, .T. ) ;
#9967 = CARTESIAN_POINT ( 'NONE',  ( -46.99999999999988631, 559.9933750504617365, -560.4184312811007658 ) ) ;
#9968 = ORIENTED_EDGE ( 'NONE', *, *, #8352, .T. ) ;
#9969 = CARTESIAN_POINT ( 'NONE',  ( -2.216159785453297477E-13, 104.2500000000000142, 0.000000000000000000 ) ) ;
#9970 = CARTESIAN_POINT ( 'NONE',  ( -45.00000000000000000, 515.4878487013597805, -546.7230258972048205 ) ) ;
#9971 = VERTEX_POINT ( 'NONE', #1076 ) ;
#9972 = ORIENTED_EDGE ( 'NONE', *, *, #7610, .F. ) ;
#9973 = VECTOR ( 'NONE', #7913, 1000.000000000000114 ) ;
#9974 = CARTESIAN_POINT ( 'NONE',  ( -22.00000000000001776, 6.000000000000000000, 32.00000000000000711 ) ) ;
#9975 = EDGE_CURVE ( 'NONE', #4897, #16617, #14481, .T. ) ;
#9976 = APPLICATION_PROTOCOL_DEFINITION ( 'draft international standard', 'automotive_design', 1998, #76 ) ;
#9977 = AXIS2_PLACEMENT_3D ( 'NONE', #12142, #3131, #6799 ) ;
#9978 = AXIS2_PLACEMENT_3D ( 'NONE', #13955, #12494, #11203 ) ;
#9979 =( NAMED_UNIT ( * ) SI_UNIT ( $, .STERADIAN. ) SOLID_ANGLE_UNIT ( ) );
#9980 = AXIS2_PLACEMENT_3D ( 'NONE', #4165, #11200, #8459 ) ;
#9981 = CARTESIAN_POINT ( 'NONE',  ( 2.999999999999998668, 60.19942049011861940, 9.013878188659973034 ) ) ;
#9982 = ORIENTED_EDGE ( 'NONE', *, *, #2015, .T. ) ;
#9983 = DIRECTION ( 'NONE',  ( 1.000000000000000000, 0.000000000000000000, 0.000000000000000000 ) ) ;
#9984 = CARTESIAN_POINT ( 'NONE',  ( 37.50000000000000000, 196.3050121726289206, -75.00000000000000000 ) ) ;
#9985 = AXIS2_PLACEMENT_3D ( 'NONE', #8, #15632, #14350 ) ;
#9986 = ORIENTED_EDGE ( 'NONE', *, *, #11191, .T. ) ;
#9987 = FACE_OUTER_BOUND ( 'NONE', #5330, .T. ) ;
#9988 = DIRECTION ( 'NONE',  ( -0.000000000000000000, -1.000000000000000000, -0.000000000000000000 ) ) ;
#9989 = ORIENTED_EDGE ( 'NONE', *, *, #7286, .T. ) ;
#9990 = AXIS2_PLACEMENT_3D ( 'NONE', #5946, #3291, #15051 ) ;
#9991 = CARTESIAN_POINT ( 'NONE',  ( 31.00000000000002842, 0.000000000000000000, 26.00000000000001066 ) ) ;
#9992 = AXIS2_PLACEMENT_3D ( 'NONE', #3031, #5424, #4330 ) ;
#9993 = ORIENTED_EDGE ( 'NONE', *, *, #16214, .F. ) ;
#9994 = ORIENTED_EDGE ( 'NONE', *, *, #3237, .T. ) ;
#9995 = VECTOR ( 'NONE', #7078, 1000.000000000000000 ) ;
#9996 = ORIENTED_EDGE ( 'NONE', *, *, #808, .T. ) ;
#9997 = AXIS2_PLACEMENT_3D ( 'NONE', #14864, #3351, #8758 ) ;
#9998 = EDGE_LOOP ( 'NONE', ( #5447, #6769, #13361, #4403 ) ) ;
#9999 = ORIENTED_EDGE ( 'NONE', *, *, #11783, .F. ) ;
#10000 = CARTESIAN_POINT ( 'NONE',  ( 0.000000000000000000, 26.00000000000000000, 0.000000000000000000 ) ) ;
#10001 = LINE ( 'NONE', #15061, #10451 ) ;
#10002 = CARTESIAN_POINT ( 'NONE',  ( 1.574999999999999956, -14.92500000000000071, -1.827785347727424768E-15 ) ) ;
#10003 = CARTESIAN_POINT ( 'NONE',  ( -31.81980515339462912, 0.000000000000000000, 35.11980515339465825 ) ) ;
#10004 = AXIS2_PLACEMENT_3D ( 'NONE', #4561, #8766, #15213 ) ;
#10005 = CARTESIAN_POINT ( 'NONE',  ( 0.7365999999999666148, 264.4632308570089663, 287.5298983642207986 ) ) ;
#10006 = CARTESIAN_POINT ( 'NONE',  ( 26.00000000000000355, 19.00000000000000000, -31.00000000000004263 ) ) ;
#10007 = EDGE_CURVE ( 'NONE', #9971, #15562, #10433, .T. ) ;
#10008 = FACE_OUTER_BOUND ( 'NONE', #14226, .T. ) ;
#10009 = FACE_BOUND ( 'NONE', #6370, .T. ) ;
#10010 = ORIENTED_EDGE ( 'NONE', *, *, #15649, .F. ) ;
#10011 = DIRECTION ( 'NONE',  ( -1.000000000000000000, -0.000000000000000000, -0.000000000000000000 ) ) ;
#10012 = DIRECTION ( 'NONE',  ( 0.000000000000000000, 0.000000000000000000, -1.000000000000000000 ) ) ;
#10013 = VERTEX_POINT ( 'NONE', #16857 ) ;
#10014 = DIRECTION ( 'NONE',  ( -1.000000000000000000, -0.000000000000000000, -0.000000000000000000 ) ) ;
#10016 = VERTEX_POINT ( 'NONE', #7933 ) ;
#10015 = ORIENTED_EDGE ( 'NONE', *, *, #14747, .T. ) ;
#10017 = EDGE_CURVE ( 'NONE', #9826, #6948, #6324, .T. ) ;
#10018 = CARTESIAN_POINT ( 'NONE',  ( -0.9999999999999991118, 0.000000000000000000, 0.000000000000000000 ) ) ;
#10019 = AXIS2_PLACEMENT_3D ( 'NONE', #9953, #2123, #769 ) ;
#10020 = EDGE_LOOP ( 'NONE', ( #1214, #13618, #8842, #12888 ) ) ;
#10021 = DIRECTION ( 'NONE',  ( 0.000000000000000000, 0.000000000000000000, -1.000000000000000000 ) ) ;
#10022 = LINE ( 'NONE', #2193, #23 ) ;
#10023 = CYLINDRICAL_SURFACE ( 'NONE', #2007, 84.99999999999997158 ) ;
#10024 = ORIENTED_EDGE ( 'NONE', *, *, #12363, .T. ) ;
#10025 = UNCERTAINTY_MEASURE_WITH_UNIT (LENGTH_MEASURE( 1.000000000000000082E-05 ), #1452, 'distance_accuracy_value', 'NONE');
#10026 = CARTESIAN_POINT ( 'NONE',  ( 0.000000000000000000, 0.000000000000000000, 0.000000000000000000 ) ) ;
#10027 = DIRECTION ( 'NONE',  ( 0.000000000000000000, 0.000000000000000000, 1.000000000000000000 ) ) ;
#10029 = ADVANCED_FACE ( 'NONE', ( #2440 ), #7975, .T. ) ;
#10028 = ORIENTED_EDGE ( 'NONE', *, *, #12849, .F. ) ;
#10030 = DIRECTION ( 'NONE',  ( 0.000000000000000000, 0.000000000000000000, -1.000000000000000000 ) ) ;
#10031 = CIRCLE ( 'NONE', #8925, 9.000000000000007105 ) ;
#10032 = DIRECTION ( 'NONE',  ( -0.000000000000000000, -1.000000000000000000, -0.000000000000000000 ) ) ;
#10033 = CARTESIAN_POINT ( 'NONE',  ( -45.00000000000000000, 523.2161522479893847, -590.5524132976893270 ) ) ;
#10034 = DIRECTION ( 'NONE',  ( -0.000000000000000000, -1.000000000000000000, -0.000000000000000000 ) ) ;
#10035 = CARTESIAN_POINT ( 'NONE',  ( 31.00000000000001776, 0.000000000000000000, -25.99999999999999645 ) ) ;
#10036 = VERTEX_POINT ( 'NONE', #15663 ) ;
#10037 = EDGE_CURVE ( 'NONE', #14546, #4127, #10186, .T. ) ;
#10038 = ADVANCED_FACE ( 'NONE', ( #14297 ), #5178, .T. ) ;
#10039 = CYLINDRICAL_SURFACE ( 'NONE', #10019, 25.00000000000002132 ) ;
#10040 = EDGE_CURVE ( 'NONE', #14998, #963, #3055, .T. ) ;
#10041 = VECTOR ( 'NONE', #15387, 1000.000000000000000 ) ;
#10042 = DIRECTION ( 'NONE',  ( 0.000000000000000000, 0.000000000000000000, 1.000000000000000000 ) ) ;
#10043 = FACE_OUTER_BOUND ( 'NONE', #4741, .T. ) ;
#10044 = ORIENTED_EDGE ( 'NONE', *, *, #13682, .F. ) ;
#10045 = FACE_OUTER_BOUND ( 'NONE', #6704, .T. ) ;
#10046 = DIRECTION ( 'NONE',  ( 0.000000000000000000, 0.000000000000000000, 1.000000000000000000 ) ) ;
#10047 = ORIENTED_EDGE ( 'NONE', *, *, #3803, .T. ) ;
#10048 = LINE ( 'NONE', #9878, #6965 ) ;
#10049 = CARTESIAN_POINT ( 'NONE',  ( -40.00000000000000711, 10.00000000000000000, 26.00000000000000000 ) ) ;
#10050 = CARTESIAN_POINT ( 'NONE',  ( 31.00000000000000000, 19.00000000000000000, -31.00000000000000355 ) ) ;
#10051 = EDGE_LOOP ( 'NONE', ( #9107, #3535, #15057, #11754, #10912, #11602 ) ) ;
#10052 = VECTOR ( 'NONE', #14789, 1000.000000000000000 ) ;
#10053 = AXIS2_PLACEMENT_3D ( 'NONE', #697, #855, #8756 ) ;
#10054 = FILL_AREA_STYLE_COLOUR ( '', #9061 ) ;
#10055 = CARTESIAN_POINT ( 'NONE',  ( -55.99999999999989342, 549.5810598491749488, -589.0260321808809749 ) ) ;
#10056 = DIRECTION ( 'NONE',  ( -0.000000000000000000, -0.000000000000000000, 1.000000000000000000 ) ) ;
#10057 = ORIENTED_EDGE ( 'NONE', *, *, #12760, .F. ) ;
#10058 = EDGE_CURVE ( 'NONE', #544, #15036, #12648, .T. ) ;
#10059 = ORIENTED_EDGE ( 'NONE', *, *, #3540, .F. ) ;
#10060 = EDGE_CURVE ( 'NONE', #2088, #9116, #9761, .T. ) ;
#10061 = CARTESIAN_POINT ( 'NONE',  ( 415.0210210471910841, 329.6061121441327941, -6.736600000000000144 ) ) ;
#10062 = EDGE_CURVE ( 'NONE', #11116, #3377, #12070, .T. ) ;
#10063 = SHAPE_DEFINITION_REPRESENTATION ( #6553, #25 ) ;
#10064 = SHAPE_REPRESENTATION_RELATIONSHIP ( 'NONE' , 'NONE' ,  #5843, #11793 ) ;
#10065 = CARTESIAN_POINT ( 'NONE',  ( 0.000000000000000000, 66.00000000000000000, -5.741599279633704455E-16 ) ) ;
#10066 = AXIS2_PLACEMENT_3D ( 'NONE', #7962, #1618, #1797 ) ;
#10067 = VERTEX_POINT ( 'NONE', #11031 ) ;
#10068 = AXIS2_PLACEMENT_3D ( 'NONE', #12515, #8406, #11224 ) ;
#10069 = CARTESIAN_POINT ( 'NONE',  ( 10.00000000000000000, 185.0000000000000284, -206.3519347178565795 ) ) ;
#10070 = DIRECTION ( 'NONE',  ( -0.000000000000000000, -1.000000000000000000, -0.000000000000000000 ) ) ;
#10071 = ORIENTED_EDGE ( 'NONE', *, *, #10641, .T. ) ;
#10072 = CARTESIAN_POINT ( 'NONE',  ( -35.00000000000000000, 19.00000000000000000, -21.00000000000000000 ) ) ;
#10073 = DIRECTION ( 'NONE',  ( 0.000000000000000000, 0.000000000000000000, -1.000000000000000000 ) ) ;
#10074 = ORIENTED_EDGE ( 'NONE', *, *, #10323, .T. ) ;
#10075 = CYLINDRICAL_SURFACE ( 'NONE', #9990, 0.7365999999986965197 ) ;
#10076 = ORIENTED_EDGE ( 'NONE', *, *, #4283, .F. ) ;
#10077 = ORIENTED_EDGE ( 'NONE', *, *, #477, .F. ) ;
#10078 = VECTOR ( 'NONE', #33, 1000.000000000000000 ) ;
#10079 = ORIENTED_EDGE ( 'NONE', *, *, #5842, .F. ) ;
#10080 =( NAMED_UNIT ( * ) SI_UNIT ( $, .STERADIAN. ) SOLID_ANGLE_UNIT ( ) );
#10081 = EDGE_LOOP ( 'NONE', ( #15897, #7772 ) ) ;
#10082 = EDGE_LOOP ( 'NONE', ( #1725, #8554 ) ) ;
#10083 = CARTESIAN_POINT ( 'NONE',  ( -26.00000000000002132, 10.00000000000000000, -31.00000000000003553 ) ) ;
#10084 = CARTESIAN_POINT ( 'NONE',  ( 39.06972645625037899, 346.7108172824755457, 0.000000000000000000 ) ) ;
#10085 = CARTESIAN_POINT ( 'NONE',  ( -37.00000000000000000, 68.00000000000000000, 23.00000000000000355 ) ) ;
#10086 = DIRECTION ( 'NONE',  ( -0.000000000000000000, -1.000000000000000000, -0.000000000000000000 ) ) ;
#10087 = LINE ( 'NONE', #16681, #4207 ) ;
#10088 = DIRECTION ( 'NONE',  ( 0.000000000000000000, -0.9227698650333863162, 0.3853514969300962378 ) ) ;
#10089 = ADVANCED_FACE ( 'NONE', ( #5788 ), #14901, .T. ) ;
#10090 = DIRECTION ( 'NONE',  ( -0.000000000000000000, 0.000000000000000000, 1.000000000000000000 ) ) ;
#10091 = PLANE ( 'NONE',  #11866 ) ;
#10092 = ORIENTED_EDGE ( 'NONE', *, *, #10168, .F. ) ;
#10093 = DIRECTION ( 'NONE',  ( 1.000000000000000000, 0.000000000000000000, 0.000000000000000000 ) ) ;
#10094 = DIRECTION ( 'NONE',  ( 0.000000000000000000, -0.9271838545667884235, 0.3746065934159092392 ) ) ;
#10095 = FACE_OUTER_BOUND ( 'NONE', #2059, .T. ) ;
#10097 = VERTEX_POINT ( 'NONE', #14820 ) ;
#10096 = ORIENTED_EDGE ( 'NONE', *, *, #14571, .T. ) ;
#10098 = AXIS2_PLACEMENT_3D ( 'NONE', #3423, #11150, #15351 ) ;
#10099 = DIRECTION ( 'NONE',  ( 0.000000000000000000, -0.000000000000000000, 1.000000000000000000 ) ) ;
#10100 = AXIS2_PLACEMENT_3D ( 'NONE', #4218, #3013, #13333 ) ;
#10101 = ORIENTED_EDGE ( 'NONE', *, *, #6559, .F. ) ;
#10102 = PRODUCT_DEFINITION ( 'UNKNOWN', '', #5617, #15968 ) ;
#10103 = DIRECTION ( 'NONE',  ( 0.000000000000000000, 1.000000000000000000, 0.000000000000000000 ) ) ;
#10104 = FACE_OUTER_BOUND ( 'NONE', #3028, .T. ) ;
#10105 = ORIENTED_EDGE ( 'NONE', *, *, #6174, .T. ) ;
#10106 = DIRECTION ( 'NONE',  ( 1.000000000000000000, -0.000000000000000000, -0.000000000000000000 ) ) ;
#10107 = ADVANCED_FACE ( 'NONE', ( #13624 ), #16270, .T. ) ;
#10108 = DIRECTION ( 'NONE',  ( 1.000000000000000000, 0.000000000000000000, 0.000000000000000000 ) ) ;
#10109 = ORIENTED_EDGE ( 'NONE', *, *, #9975, .F. ) ;
#10110 = DIRECTION ( 'NONE',  ( -1.000000000000000000, -0.000000000000000000, -1.631319816340925608E-17 ) ) ;
#10111 = AXIS2_PLACEMENT_3D ( 'NONE', #16477, #12371, #11167 ) ;
#10112 = DIRECTION ( 'NONE',  ( -1.000000000000000000, -0.000000000000000000, -0.000000000000000000 ) ) ;
#10113 = CARTESIAN_POINT ( 'NONE',  ( 5.687501635565830327, 0.000000000000000000, 0.000000000000000000 ) ) ;
#10114 = PLANE ( 'NONE',  #13253 ) ;
#10115 = CARTESIAN_POINT ( 'NONE',  ( -31.00000000000002132, 10.00000000000000000, -31.00000000000000000 ) ) ;
#10116 = ORIENTED_EDGE ( 'NONE', *, *, #7309, .T. ) ;
#10117 = DIRECTION ( 'NONE',  ( -0.000000000000000000, 0.000000000000000000, -1.000000000000000000 ) ) ;
#10118 = PLANE ( 'NONE',  #4700 ) ;
#10119 = ADVANCED_FACE ( 'NONE', ( #1771 ), #12158, .T. ) ;
#10120 = FACE_OUTER_BOUND ( 'NONE', #16088, .T. ) ;
#10121 = VERTEX_POINT ( 'NONE', #3226 ) ;
#10122 = FACE_OUTER_BOUND ( 'NONE', #5012, .T. ) ;
#10123 = EDGE_CURVE ( 'NONE', #13274, #1501, #1405, .T. ) ;
#10124 = ADVANCED_FACE ( 'NONE', ( #4348 ), #13452, .T. ) ;
#10125 = AXIS2_PLACEMENT_3D ( 'NONE', #8819, #15520, #3671 ) ;
#10126 = CARTESIAN_POINT ( 'NONE',  ( -55.99999999999989342, 549.5810598491749488, -575.3306267969850296 ) ) ;
#10127 = ORIENTED_EDGE ( 'NONE', *, *, #7160, .T. ) ;
#10128 = CARTESIAN_POINT ( 'NONE',  ( 0.3499999999999999778, 0.000000000000000000, 0.000000000000000000 ) ) ;
#10129 = ADVANCED_FACE ( 'NONE', ( #16181 ), #5530, .F. ) ;
#10130 = CARTESIAN_POINT ( 'NONE',  ( -25.99999999999999645, 68.00000000000000000, -31.00000000000003197 ) ) ;
#10131 = DIRECTION ( 'NONE',  ( 0.000000000000000000, 0.000000000000000000, 1.000000000000000000 ) ) ;
#10132 = ORIENTED_EDGE ( 'NONE', *, *, #2792, .F. ) ;
#10133 = PRODUCT ( 'TAS-007', 'TAS-007', '', ( #10582 ) ) ;
#10134 = DIRECTION ( 'NONE',  ( -0.000000000000000000, -1.000000000000000000, -0.000000000000000000 ) ) ;
#10135 = CARTESIAN_POINT ( 'NONE',  ( -26.00000000000001776, 10.00000000000000000, 31.00000000000003553 ) ) ;
#10136 = CARTESIAN_POINT ( 'NONE',  ( 394.0000000000001137, 341.4647406485092915, -16.00114864346762644 ) ) ;
#10137 = ORIENTED_EDGE ( 'NONE', *, *, #6894, .T. ) ;
#10138 = DIRECTION ( 'NONE',  ( -0.000000000000000000, 0.000000000000000000, 1.000000000000000000 ) ) ;
#10139 = VECTOR ( 'NONE', #2070, 1000.000000000000000 ) ;
#10140 = SHAPE_REPRESENTATION_RELATIONSHIP ( 'NONE' , 'NONE' ,  #1329, #15527 ) ;
#10141 = ADVANCED_FACE ( 'NONE', ( #3051 ), #6731, .T. ) ;
#10142 = LINE ( 'NONE', #6570, #1380 ) ;
#10143 = ORIENTED_EDGE ( 'NONE', *, *, #2455, .T. ) ;
#10144 = CARTESIAN_POINT ( 'NONE',  ( 31.00000000000000000, 8.000000000000000000, -31.00000000000000355 ) ) ;
#10145 = ADVANCED_FACE ( 'NONE', ( #11987 ), #9671, .T. ) ;
#10146 = DIRECTION ( 'NONE',  ( -1.000000000000000000, -0.000000000000000000, -0.000000000000000000 ) ) ;
#10147 = ADVANCED_FACE ( 'NONE', ( #10691 ), #15924, .T. ) ;
#10148 = EDGE_CURVE ( 'NONE', #2164, #12818, #2878, .T. ) ;
#10149 = EDGE_LOOP ( 'NONE', ( #15211, #1225, #13000, #6881 ) ) ;
#10150 = DIRECTION ( 'NONE',  ( 1.000000000000000000, -0.000000000000000000, 0.000000000000000000 ) ) ;
#10151 = EDGE_CURVE ( 'NONE', #6355, #1812, #9499, .T. ) ;
#10152 = LINE ( 'NONE', #15308, #14425 ) ;
#10153 = ORIENTED_EDGE ( 'NONE', *, *, #11101, .F. ) ;
#10154 = VECTOR ( 'NONE', #494, 1000.000000000000000 ) ;
#10155 = DIRECTION ( 'NONE',  ( 0.000000000000000000, 0.000000000000000000, 1.000000000000000000 ) ) ;
#10156 = ORIENTED_EDGE ( 'NONE', *, *, #10365, .T. ) ;
#10157 = ORIENTED_EDGE ( 'NONE', *, *, #6686, .F. ) ;
#10158 = VECTOR ( 'NONE', #4962, 1000.000000000000000 ) ;
#10159 = ORIENTED_EDGE ( 'NONE', *, *, #6437, .F. ) ;
#10160 = ORIENTED_EDGE ( 'NONE', *, *, #1200, .T. ) ;
#10161 = CIRCLE ( 'NONE', #15635, 9.000000000000007105 ) ;
#10162 = ORIENTED_EDGE ( 'NONE', *, *, #11613, .F. ) ;
#10163 = CIRCLE ( 'NONE', #14004, 4.695405383896011919 ) ;
#10164 = LINE ( 'NONE', #2172, #15393 ) ;
#10165 = DIRECTION ( 'NONE',  ( -0.000000000000000000, 0.09950371902100807464, -0.9950371902099882648 ) ) ;
#10166 = CYLINDRICAL_SURFACE ( 'NONE', #4347, 6.473200000000000287 ) ;
#10167 = DIRECTION ( 'NONE',  ( 1.000000000000000000, 0.000000000000000000, 0.000000000000000000 ) ) ;
#10168 = EDGE_CURVE ( 'NONE', #10736, #11828, #8716, .T. ) ;
#10169 = CARTESIAN_POINT ( 'NONE',  ( -26.00000000000000000, 11.00000000000000000, 40.00000000000000711 ) ) ;
#10170 = CARTESIAN_POINT ( 'NONE',  ( 0.000000000000000000, 0.000000000000000000, -34.00000000000000000 ) ) ;
#10171 = DIRECTION ( 'NONE',  ( 0.000000000000000000, 0.000000000000000000, -1.000000000000000000 ) ) ;
#10172 = ORIENTED_EDGE ( 'NONE', *, *, #8927, .T. ) ;
#10173 = DIRECTION ( 'NONE',  ( 0.000000000000000000, 1.000000000000000000, 0.000000000000000000 ) ) ;
#10174 = CARTESIAN_POINT ( 'NONE',  ( 31.00000000000006395, 0.000000000000000000, -22.99999999999999289 ) ) ;
#10175 = ORIENTED_EDGE ( 'NONE', *, *, #463, .F. ) ;
#10176 = TOROIDAL_SURFACE ( 'NONE', #13747, 4.695405383895982609, 9.000000000000000000 ) ;
#10177 = DIRECTION ( 'NONE',  ( 1.000000000000000000, -0.000000000000000000, 0.000000000000000000 ) ) ;
#10179 = VERTEX_POINT ( 'NONE', #10084 ) ;
#10178 = ORIENTED_EDGE ( 'NONE', *, *, #6249, .F. ) ;
#10180 =( REPRESENTATION_RELATIONSHIP ('NONE','NONE', #15277, #9356 ) REPRESENTATION_RELATIONSHIP_WITH_TRANSFORMATION ( #15376 )SHAPE_REPRESENTATION_RELATIONSHIP( ) );
#10181 = DIRECTION ( 'NONE',  ( 0.000000000000000000, 0.000000000000000000, -1.000000000000000000 ) ) ;
#10182 = EDGE_CURVE ( 'NONE', #11977, #15142, #3302, .T. ) ;
#10183 =( NAMED_UNIT ( * ) PLANE_ANGLE_UNIT ( ) SI_UNIT ( $, .RADIAN. ) );
#10184 = LINE ( 'NONE', #13798, #6872 ) ;
#10185 = DIRECTION ( 'NONE',  ( -0.000000000000000000, 1.000000000000000000, -0.000000000000000000 ) ) ;
#10186 = CIRCLE ( 'NONE', #4429, 3.000000000000002665 ) ;
#10187 = EDGE_LOOP ( 'NONE', ( #9945, #1050, #16309, #6543 ) ) ;
#10188 = UNCERTAINTY_MEASURE_WITH_UNIT (LENGTH_MEASURE( 1.000000000000000082E-05 ), #15301, 'distance_accuracy_value', 'NONE');
#10189 = CARTESIAN_POINT ( 'NONE',  ( 37.00000000000000000, 68.00000000000000000, 23.00000000000001066 ) ) ;
#10190 = CYLINDRICAL_SURFACE ( 'NONE', #8697, 6.473199999999998511 ) ;
#10191 = ORIENTED_EDGE ( 'NONE', *, *, #498, .T. ) ;
#10192 = FACE_OUTER_BOUND ( 'NONE', #3309, .T. ) ;
#10193 = VECTOR ( 'NONE', #2993, 1000.000000000000000 ) ;
#10194 = DIRECTION ( 'NONE',  ( -1.000000000000000000, -0.000000000000000000, -0.000000000000000000 ) ) ;
#10195 = CYLINDRICAL_SURFACE ( 'NONE', #12944, 13.69540538389601991 ) ;
#10196 = LINE ( 'NONE', #12934, #16038 ) ;
#10197 = CARTESIAN_POINT ( 'NONE',  ( -22.99999999999999645, 68.00000000000000000, 31.00000000000003908 ) ) ;
#10198 = EDGE_LOOP ( 'NONE', ( #2100, #6187, #8571, #7115 ) ) ;
#10199 = CIRCLE ( 'NONE', #2787, 34.00000000000000000 ) ;
#10200 = DIRECTION ( 'NONE',  ( -1.000000000000000000, -0.000000000000000000, -0.000000000000000000 ) ) ;
#10201 = AXIS2_PLACEMENT_3D ( 'NONE', #3859, #9190, #1453 ) ;
#10202 = DIRECTION ( 'NONE',  ( 0.000000000000000000, -0.000000000000000000, 1.000000000000000000 ) ) ;
#10203 = CIRCLE ( 'NONE', #6068, 4.999999999999997335 ) ;
#10204 = CIRCLE ( 'NONE', #1976, 2.999999999999999112 ) ;
#10205 = CARTESIAN_POINT ( 'NONE',  ( -34.99999999999998579, 3.000000000000000000, 18.50000000000000355 ) ) ;
#10206 = ORIENTED_EDGE ( 'NONE', *, *, #7866, .F. ) ;
#10207 = CARTESIAN_POINT ( 'NONE',  ( 394.0000000000001137, 240.7889724647196488, -104.9456657433598110 ) ) ;
#10208 = CIRCLE ( 'NONE', #15146, 8.000000000000000000 ) ;
#10209 = DIRECTION ( 'NONE',  ( 0.000000000000000000, 0.000000000000000000, -1.000000000000000000 ) ) ;
#10210 = ORIENTED_EDGE ( 'NONE', *, *, #13017, .T. ) ;
#10211 = CARTESIAN_POINT ( 'NONE',  ( -22.99999999999999645, 68.00000000000000000, -36.99999999999999289 ) ) ;
#10212 = DIRECTION ( 'NONE',  ( 1.000000000000000000, 0.000000000000000000, 0.000000000000000000 ) ) ;
#10213 = CARTESIAN_POINT ( 'NONE',  ( -5.000000000000000888, 0.000000000000000000, 0.000000000000000000 ) ) ;
#10214 = EDGE_LOOP ( 'NONE', ( #8508, #15651, #3196, #7782 ) ) ;
#10215 = EDGE_CURVE ( 'NONE', #8625, #8747, #325, .T. ) ;
#10216 = DIRECTION ( 'NONE',  ( -0.000000000000000000, 1.000000000000000000, -0.000000000000000000 ) ) ;
#10217 = CIRCLE ( 'NONE', #2519, 29.99999999999530687 ) ;
#10218 = CARTESIAN_POINT ( 'NONE',  ( -0.3121190734747608664, 289.3528227838038447, 37.58596727633977963 ) ) ;
#10219 = EDGE_LOOP ( 'NONE', ( #12317, #8081, #7357, #9029 ) ) ;
#10220 = DIRECTION ( 'NONE',  ( 0.000000000000000000, 0.000000000000000000, 1.000000000000000000 ) ) ;
#10221 = CONTEXT_DEPENDENT_SHAPE_REPRESENTATION ( #11055, #9326 ) ;
#10222 = VECTOR ( 'NONE', #1442, 1000.000000000000000 ) ;
#10223 = EDGE_CURVE ( 'NONE', #4822, #10494, #10001, .T. ) ;
#10224 = SHAPE_REPRESENTATION_RELATIONSHIP ( 'NONE' , 'NONE' ,  #6937, #556 ) ;
#10225 = VERTEX_POINT ( 'NONE', #4656 ) ;
#10226 = COLOUR_RGB ( '', 0.72549020, 0.75294118, 0.79215686) ;
#10227 = CARTESIAN_POINT ( 'NONE',  ( 18.99999999999998224, 8.000000000000000000, -35.99999999999999289 ) ) ;
#10228 = CARTESIAN_POINT ( 'NONE',  ( 10.00000000000000000, 341.0487089519837696, -115.0000000000032969 ) ) ;
#10229 = CARTESIAN_POINT ( 'NONE',  ( 30.99999999999999645, 3.000000000000000000, -25.99999999999999645 ) ) ;
#10230 = ORIENTED_EDGE ( 'NONE', *, *, #16926, .T. ) ;
#10231 = CARTESIAN_POINT ( 'NONE',  ( 25.99999999999997868, 0.000000000000000000, 40.00000000000000711 ) ) ;
#10232 = CARTESIAN_POINT ( 'NONE',  ( -39.99999999999999289, 8.000000000000000000, 34.99999999999997868 ) ) ;
#10233 = ORIENTED_EDGE ( 'NONE', *, *, #4582, .T. ) ;
#10234 = VECTOR ( 'NONE', #9744, 1000.000000000000000 ) ;
#10235 = EDGE_CURVE ( 'NONE', #2243, #14813, #36, .T. ) ;
#10236 = CARTESIAN_POINT ( 'NONE',  ( -55.99999999999989342, 493.2350855268092573, -585.2659423243250103 ) ) ;
#10237 = ORIENTED_EDGE ( 'NONE', *, *, #13513, .T. ) ;
#10238 = ORIENTED_EDGE ( 'NONE', *, *, #11360, .F. ) ;
#10239 = CARTESIAN_POINT ( 'NONE',  ( 3.000000000000000000, 6.000000000000000000, 22.00000000000000000 ) ) ;
#10240 = CIRCLE ( 'NONE', #1186, 13.69540538389597017 ) ;
#10241 = VECTOR ( 'NONE', #1665, 1000.000000000000000 ) ;
#10242 = CIRCLE ( 'NONE', #7212, 3.000000000000002665 ) ;
#10243 = ORIENTED_EDGE ( 'NONE', *, *, #2090, .T. ) ;
#10244 = EDGE_CURVE ( 'NONE', #8973, #9661, #13697, .T. ) ;
#10245 = CARTESIAN_POINT ( 'NONE',  ( 0.000000000000000000, 0.000000000000000000, 0.000000000000000000 ) ) ;
#10246 = EDGE_CURVE ( 'NONE', #9815, #5137, #7401, .T. ) ;
#10247 = EDGE_CURVE ( 'NONE', #14244, #11248, #9646, .T. ) ;
#10248 = EDGE_CURVE ( 'NONE', #1605, #12055, #11365, .T. ) ;
#10249 = ORIENTED_EDGE ( 'NONE', *, *, #10444, .T. ) ;
#10250 = AXIS2_PLACEMENT_3D ( 'NONE', #15225, #11182, #16416 ) ;
#10251 = ORIENTED_EDGE ( 'NONE', *, *, #6579, .T. ) ;
#10252 = LINE ( 'NONE', #11614, #1966 ) ;
#10253 = DIRECTION ( 'NONE',  ( -0.000000000000000000, -1.000000000000000000, -0.000000000000000000 ) ) ;
#10254 = VECTOR ( 'NONE', #12481, 1000.000000000000000 ) ;
#10255 = AXIS2_PLACEMENT_3D ( 'NONE', #6120, #11122, #9838 ) ;
#10256 = CARTESIAN_POINT ( 'NONE',  ( 394.0000000000001137, 339.1725919290087745, -9.945665743359786148 ) ) ;
#10257 = CARTESIAN_POINT ( 'NONE',  ( -23.00000000000003197, 0.000000000000000000, 37.00000000000000711 ) ) ;
#10258 = AXIS2_PLACEMENT_3D ( 'NONE', #5084, #7479, #14031 ) ;
#10259 = PLANE ( 'NONE',  #109 ) ;
#10260 = DIRECTION ( 'NONE',  ( -0.000000000000000000, -0.000000000000000000, 1.000000000000000000 ) ) ;
#10261 = VECTOR ( 'NONE', #6602, 1000.000000000000000 ) ;
#10262 = DIRECTION ( 'NONE',  ( -1.000000000000000000, -0.000000000000000000, -0.000000000000000000 ) ) ;
#10263 = VERTEX_POINT ( 'NONE', #11447 ) ;
#10264 = PLANE ( 'NONE',  #13652 ) ;
#10265 = DIRECTION ( 'NONE',  ( 0.000000000000000000, 0.000000000000000000, 1.000000000000000000 ) ) ;
#10266 = CIRCLE ( 'NONE', #4505, 13.69540538389601991 ) ;
#10267 = ORIENTED_EDGE ( 'NONE', *, *, #4064, .F. ) ;
#10268 = CARTESIAN_POINT ( 'NONE',  ( -23.00000000000003197, 3.000000000000000000, 34.00000000000000711 ) ) ;
#10270 = ORIENTED_EDGE ( 'NONE', *, *, #2677, .F. ) ;
#10269 = EDGE_LOOP ( 'NONE', ( #6262, #10993, #888, #6140 ) ) ;
#10271 = EDGE_CURVE ( 'NONE', #1746, #14275, #10164, .T. ) ;
#10272 = ADVANCED_FACE ( 'NONE', ( #891 ), #7235, .T. ) ;
#10273 = CARTESIAN_POINT ( 'NONE',  ( 30.99999999999999645, 68.00000000000000000, 26.00000000000001066 ) ) ;
#10274 = EDGE_CURVE ( 'NONE', #7469, #8018, #15119, .T. ) ;
#10275 = VECTOR ( 'NONE', #16163, 1000.000000000000000 ) ;
#10276 = EDGE_LOOP ( 'NONE', ( #10378, #6323 ) ) ;
#10277 = ORIENTED_EDGE ( 'NONE', *, *, #3213, .F. ) ;
#10278 = DIRECTION ( 'NONE',  ( 1.000000000000000000, 0.000000000000000000, 0.000000000000000000 ) ) ;
#10279 = VECTOR ( 'NONE', #617, 1000.000000000000000 ) ;
#10280 = DIRECTION ( 'NONE',  ( 1.000000000000000000, 0.000000000000000000, -0.000000000000000000 ) ) ;
#10281 = LINE ( 'NONE', #16700, #15451 ) ;
#10282 = VERTEX_POINT ( 'NONE', #15144 ) ;
#10283 = PRODUCT ( 'Part6', 'Part6', '', ( #3025 ) ) ;
#10284 = DIRECTION ( 'NONE',  ( -0.000000000000000000, -1.000000000000000000, -0.000000000000000000 ) ) ;
#10285 = ORIENTED_EDGE ( 'NONE', *, *, #16846, .T. ) ;
#10286 = LINE ( 'NONE', #3918, #14269 ) ;
#10287 = AXIS2_PLACEMENT_3D ( 'NONE', #11812, #3668, #2625 ) ;
#10288 = CARTESIAN_POINT ( 'NONE',  ( 0.03302700000123198060, 193.4898140233673018, 37.52989836422092651 ) ) ;
#10289 = DIRECTION ( 'NONE',  ( 0.000000000000000000, -0.6427876096865404731, 0.7660444431189771253 ) ) ;
#10290 = CIRCLE ( 'NONE', #13854, 18.46360580700775245 ) ;
#10291 = CARTESIAN_POINT ( 'NONE',  ( 36.99999999999999289, 10.00000000000000000, 22.99999999999999645 ) ) ;
#10292 = DIRECTION ( 'NONE',  ( -1.000000000000000000, 0.000000000000000000, 0.000000000000000000 ) ) ;
#10293 = EDGE_LOOP ( 'NONE', ( #15135, #11745, #12149, #16611 ) ) ;
#10294 = DIRECTION ( 'NONE',  ( 0.000000000000000000, 0.9271838545667883125, 0.3746065934159095168 ) ) ;
#10295 = CARTESIAN_POINT ( 'NONE',  ( 0.000000000000000000, 66.00000000000000000, 0.000000000000000000 ) ) ;
#10296 = FACE_OUTER_BOUND ( 'NONE', #14074, .T. ) ;
#10297 = VERTEX_POINT ( 'NONE', #2003 ) ;
#10298 = CIRCLE ( 'NONE', #8659, 9.500000000000000000 ) ;
#10299 = CARTESIAN_POINT ( 'NONE',  ( 0.000000000000000000, 449.3157724647197142, 33.76061909850716347 ) ) ;
#10300 = ORIENTED_EDGE ( 'NONE', *, *, #9068, .T. ) ;
#10301 = PLANE ( 'NONE',  #15208 ) ;
#10302 = CARTESIAN_POINT ( 'NONE',  ( 25.99999999999998224, 10.00000000000000000, -31.99999999999998579 ) ) ;
#10303 = DIRECTION ( 'NONE',  ( -1.000000000000000000, 0.000000000000000000, 0.000000000000000000 ) ) ;
#10304 = VERTEX_POINT ( 'NONE', #4835 ) ;
#10305 = CARTESIAN_POINT ( 'NONE',  ( -55.99999999999989342, 549.5810598491749488, -575.3306267969850296 ) ) ;
#10306 = DIRECTION ( 'NONE',  ( 0.000000000000000000, 1.000000000000000000, 0.000000000000000000 ) ) ;
#10307 = PLANE ( 'NONE',  #13222 ) ;
#10308 = ORIENTED_EDGE ( 'NONE', *, *, #10223, .F. ) ;
#10309 = VECTOR ( 'NONE', #6261, 1000.000000000000000 ) ;
#10310 = DIRECTION ( 'NONE',  ( -1.000000000000000000, -0.000000000000000000, 0.000000000000000000 ) ) ;
#10311 = AXIS2_PLACEMENT_3D ( 'NONE', #6776, #8073, #15970 ) ;
#10312 = EDGE_LOOP ( 'NONE', ( #14625, #4326, #2436, #2758 ) ) ;
#10313 = EDGE_CURVE ( 'NONE', #12863, #9277, #13218, .T. ) ;
#10314 = CARTESIAN_POINT ( 'NONE',  ( 10.00000000000000000, 376.0487089519832011, -80.00000000000332534 ) ) ;
#10315 = DIRECTION ( 'NONE',  ( -0.000000000000000000, -0.000000000000000000, 1.000000000000000000 ) ) ;
#10316 = VECTOR ( 'NONE', #4030, 1000.000000000000000 ) ;
#10317 = DIRECTION ( 'NONE',  ( 0.000000000000000000, 0.000000000000000000, 1.000000000000000000 ) ) ;
#10318 = VERTEX_POINT ( 'NONE', #3555 ) ;
#10319 = AXIS2_PLACEMENT_3D ( 'NONE', #11571, #7785, #16805 ) ;
#10320 = CARTESIAN_POINT ( 'NONE',  ( 45.00000000000000000, 493.2350855268086320, -508.1801094700848580 ) ) ;
#10321 = DIRECTION ( 'NONE',  ( 0.000000000000000000, 0.6427876096865285938, 0.7660444431189872283 ) ) ;
#10322 = EDGE_LOOP ( 'NONE', ( #6729, #13561 ) ) ;
#10323 = EDGE_CURVE ( 'NONE', #14135, #3345, #15680, .T. ) ;
#10324 = FACE_OUTER_BOUND ( 'NONE', #15380, .T. ) ;
#10325 = ORIENTED_EDGE ( 'NONE', *, *, #4060, .F. ) ;
#10326 = ORIENTED_EDGE ( 'NONE', *, *, #9274, .F. ) ;
#10327 = LINE ( 'NONE', #14109, #4770 ) ;
#10328 = ORIENTED_EDGE ( 'NONE', *, *, #1227, .F. ) ;
#10329 = DIRECTION ( 'NONE',  ( 0.000000000000000000, 0.000000000000000000, 1.000000000000000000 ) ) ;
#10330 = AXIS2_PLACEMENT_3D ( 'NONE', #6927, #9609, #10715 ) ;
#10331 = AXIS2_PLACEMENT_3D ( 'NONE', #5901, #7262, #5731 ) ;
#10332 = VERTEX_POINT ( 'NONE', #14030 ) ;
#10333 = ORIENTED_EDGE ( 'NONE', *, *, #13390, .F. ) ;
#10334 = EDGE_CURVE ( 'NONE', #4076, #5852, #15665, .T. ) ;
#10335 = ADVANCED_FACE ( 'NONE', ( #12402 ), #5875, .F. ) ;
#10336 = PLANE ( 'NONE',  #10746 ) ;
#10337 = DIRECTION ( 'NONE',  ( -0.000000000000000000, -1.000000000000000000, -0.000000000000000000 ) ) ;
#10338 = ORIENTED_EDGE ( 'NONE', *, *, #15567, .F. ) ;
#10339 = DIRECTION ( 'NONE',  ( -1.000000000000000000, 0.000000000000000000, 0.000000000000000000 ) ) ;
#10340 =( NAMED_UNIT ( * ) PLANE_ANGLE_UNIT ( ) SI_UNIT ( $, .RADIAN. ) );
#10341 = EDGE_CURVE ( 'NONE', #7341, #2045, #12490, .T. ) ;
#10342 = VECTOR ( 'NONE', #7331, 1000.000000000000000 ) ;
#10343 = EDGE_CURVE ( 'NONE', #2412, #11631, #3893, .T. ) ;
#10344 = VECTOR ( 'NONE', #12210, 1000.000000000000000 ) ;
#10345 = ADVANCED_FACE ( 'NONE', ( #6613 ), #15570, .T. ) ;
#10346 = DIRECTION ( 'NONE',  ( 1.000000000000000000, 0.000000000000000000, 0.000000000000000000 ) ) ;
#10347 = ORIENTED_EDGE ( 'NONE', *, *, #6897, .T. ) ;
#10348 = CARTESIAN_POINT ( 'NONE',  ( -37.00000000000000711, 0.000000000000000000, -23.00000000000000000 ) ) ;
#10349 = DIRECTION ( 'NONE',  ( -1.000000000000000000, -0.000000000000000000, 1.156482317317883755E-15 ) ) ;
#10350 = ORIENTED_EDGE ( 'NONE', *, *, #5587, .F. ) ;
#10351 = LINE ( 'NONE', #13011, #8519 ) ;
#10352 = ORIENTED_EDGE ( 'NONE', *, *, #1342, .F. ) ;
#10353 = FACE_BOUND ( 'NONE', #11189, .T. ) ;
#10354 = ORIENTED_EDGE ( 'NONE', *, *, #6742, .T. ) ;
#10355 = AXIS2_PLACEMENT_3D ( 'NONE', #6246, #4417, #2140 ) ;
#10356 = ORIENTED_EDGE ( 'NONE', *, *, #10442, .F. ) ;
#10357 = DIRECTION ( 'NONE',  ( 0.000000000000000000, 0.000000000000000000, -1.000000000000000000 ) ) ;
#10358 = EDGE_CURVE ( 'NONE', #1644, #1233, #15733, .T. ) ;
#10359 = CARTESIAN_POINT ( 'NONE',  ( -36.99999999999997868, 0.000000000000000000, -22.99999999999999645 ) ) ;
#10360 = CARTESIAN_POINT ( 'NONE',  ( -23.00000000000003197, 3.000000000000000000, 37.00000000000000711 ) ) ;
#10361 = ORIENTED_EDGE ( 'NONE', *, *, #13173, .T. ) ;
#10362 = CARTESIAN_POINT ( 'NONE',  ( -150.0000000000000284, 620.7506394335853201, -11.00000000000000000 ) ) ;
#10363 = DIRECTION ( 'NONE',  ( 0.000000000000000000, -0.3746065934157932764, -0.9271838545668352749 ) ) ;
#10364 = ADVANCED_FACE ( 'NONE', ( #7735 ), #9660, .T. ) ;
#10365 = EDGE_CURVE ( 'NONE', #10651, #7389, #2601, .T. ) ;
#10366 = LINE ( 'NONE', #1083, #2190 ) ;
#10367 = EDGE_CURVE ( 'NONE', #742, #12007, #3614, .T. ) ;
#10368 = DIRECTION ( 'NONE',  ( -0.000000000000000000, -0.000000000000000000, 1.000000000000000000 ) ) ;
#10369 = PLANE ( 'NONE',  #12409 ) ;
#10370 = PRESENTATION_LAYER_ASSIGNMENT (  '', '', ( #5139 ) ) ;
#10371 = DIRECTION ( 'NONE',  ( -1.000000000000000000, 0.000000000000000000, -0.000000000000000000 ) ) ;
#10372 = DIRECTION ( 'NONE',  ( 0.000000000000000000, 0.000000000000000000, 1.000000000000000000 ) ) ;
#10374 = VERTEX_POINT ( 'NONE', #7569 ) ;
#10373 = ORIENTED_EDGE ( 'NONE', *, *, #14006, .T. ) ;
#10375 = LINE ( 'NONE', #6154, #16329 ) ;
#10376 = LINE ( 'NONE', #8830, #1425 ) ;
#10377 = PLANE ( 'NONE',  #5565 ) ;
#10378 = ORIENTED_EDGE ( 'NONE', *, *, #14431, .F. ) ;
#10379 = LINE ( 'NONE', #15691, #2253 ) ;
#10380 = PLANE ( 'NONE',  #5380 ) ;
#10381 = ORIENTED_EDGE ( 'NONE', *, *, #13187, .T. ) ;
#10382 = DIRECTION ( 'NONE',  ( 1.000000000000000000, 0.000000000000000000, 0.000000000000000000 ) ) ;
#10383 = DIRECTION ( 'NONE',  ( -2.920976200236518919E-15, 0.9950371902099891530, 0.09950371902099770793 ) ) ;
#10384 = DIRECTION ( 'NONE',  ( 0.000000000000000000, 0.000000000000000000, 1.000000000000000000 ) ) ;
#10385 = VERTEX_POINT ( 'NONE', #1231 ) ;
#10386 = CARTESIAN_POINT ( 'NONE',  ( 31.81980515339464333, 11.00000000000000000, -31.81980515339463622 ) ) ;
#10387 = DIRECTION ( 'NONE',  ( -1.000000000000000000, -0.000000000000000000, -0.000000000000000000 ) ) ;
#10388 = VERTEX_POINT ( 'NONE', #118 ) ;
#10389 = DIRECTION ( 'NONE',  ( 0.000000000000000000, 0.000000000000000000, -1.000000000000000000 ) ) ;
#10390 = VECTOR ( 'NONE', #779, 1000.000000000000000 ) ;
#10391 = CONTEXT_DEPENDENT_SHAPE_REPRESENTATION ( #10498, #14397 ) ;
#10392 = EDGE_CURVE ( 'NONE', #1511, #1693, #14461, .T. ) ;
#10393 = CARTESIAN_POINT ( 'NONE',  ( 0.000000000000000000, 16.00000000000000000, -34.00000000000000000 ) ) ;
#10394 = EDGE_LOOP ( 'NONE', ( #14504, #13109, #11964, #347, #4681 ) ) ;
#10395 = DIRECTION ( 'NONE',  ( -1.000000000000000000, -0.000000000000000000, -0.000000000000000000 ) ) ;
#10396 = DIRECTION ( 'NONE',  ( -1.000000000000000000, 0.000000000000000000, -0.000000000000000000 ) ) ;
#10397 = EDGE_CURVE ( 'NONE', #14549, #9920, #12996, .T. ) ;
#10398 = CARTESIAN_POINT ( 'NONE',  ( 31.00000000000000000, 19.00000000000000000, 30.99999999999999289 ) ) ;
#10399 = EDGE_LOOP ( 'NONE', ( #12045, #413, #14886, #5646, #10381, #8556 ) ) ;
#10400 = CARTESIAN_POINT ( 'NONE',  ( 23.00000000000000711, 0.000000000000000000, -31.00000000000002487 ) ) ;
#10401 = DIRECTION ( 'NONE',  ( 1.000000000000000000, -0.000000000000000000, 0.000000000000000000 ) ) ;
#10402 = ORIENTED_EDGE ( 'NONE', *, *, #13061, .T. ) ;
#10403 = CARTESIAN_POINT ( 'NONE',  ( 1.250085104875786612E-12, 220.1329686874181562, 287.5298983642209123 ) ) ;
#10404 = VERTEX_POINT ( 'NONE', #5083 ) ;
#10405 = ORIENTED_EDGE ( 'NONE', *, *, #13509, .T. ) ;
#10406 = CARTESIAN_POINT ( 'NONE',  ( 55.99999999999989342, 523.2161522479888163, -502.8936384967199729 ) ) ;
#10407 = PRODUCT_DEFINITION ( 'UNKNOWN', '', #14678, #13413 ) ;
#10408 = ORIENTED_EDGE ( 'NONE', *, *, #16315, .T. ) ;
#10409 = VERTEX_POINT ( 'NONE', #6444 ) ;
#10410 = ADVANCED_FACE ( 'NONE', ( #6529 ), #14280, .T. ) ;
#10411 = ORIENTED_EDGE ( 'NONE', *, *, #15755, .F. ) ;
#10412 = CYLINDRICAL_SURFACE ( 'NONE', #2229, 13.69540538389601991 ) ;
#10413 = DIRECTION ( 'NONE',  ( -1.000000000000000000, -0.000000000000000000, 0.000000000000000000 ) ) ;
#10414 = AXIS2_PLACEMENT_3D ( 'NONE', #12503, #4524, #824 ) ;
#10415 = ORIENTED_EDGE ( 'NONE', *, *, #1208, .F. ) ;
#10416 = CARTESIAN_POINT ( 'NONE',  ( -22.00000000000001776, 8.000000000000000000, 33.00000000000000711 ) ) ;
#10417 = CARTESIAN_POINT ( 'NONE',  ( 46.99999999999988631, 473.6663340069157471, -531.5012393965008641 ) ) ;
#10418 = LINE ( 'NONE', #9230, #12987 ) ;
#10419 = ORIENTED_EDGE ( 'NONE', *, *, #3018, .F. ) ;
#10420 = DIRECTION ( 'NONE',  ( -0.000000000000000000, -1.000000000000000000, -0.000000000000000000 ) ) ;
#10421 = CARTESIAN_POINT ( 'NONE',  ( 17.00000000000000000, 380.0000000000000000, -75.00000000000000000 ) ) ;
#10422 = EDGE_LOOP ( 'NONE', ( #14786, #3603, #16174, #4717 ) ) ;
#10423 = ADVANCED_FACE ( 'NONE', ( #13164 ), #10412, .T. ) ;
#10424 = CARTESIAN_POINT ( 'NONE',  ( -210.0000000000000000, 512.1906115401388888, -11.00000000000000000 ) ) ;
#10425 = ORIENTED_EDGE ( 'NONE', *, *, #16123, .F. ) ;
#10426 = CARTESIAN_POINT ( 'NONE',  ( 0.000000000000000000, 16.00000000000000000, 0.000000000000000000 ) ) ;
#10427 = AXIS2_PLACEMENT_3D ( 'NONE', #6424, #7552, #5224 ) ;
#10428 = AXIS2_PLACEMENT_3D ( 'NONE', #6059, #7346, #8741 ) ;
#10429 = ORIENTED_EDGE ( 'NONE', *, *, #13721, .T. ) ;
#10430 = EDGE_CURVE ( 'NONE', #14417, #15077, #1307, .T. ) ;
#10431 = ORIENTED_EDGE ( 'NONE', *, *, #4967, .T. ) ;
#10432 = LINE ( 'NONE', #11638, #4187 ) ;
#10433 = LINE ( 'NONE', #5019, #14853 ) ;
#10434 = DIRECTION ( 'NONE',  ( 1.000000000000000000, 0.000000000000000000, 0.000000000000000000 ) ) ;
#10435 = ORIENTED_EDGE ( 'NONE', *, *, #7298, .F. ) ;
#10436 = CARTESIAN_POINT ( 'NONE',  ( 0.000000000000000000, 258.7934930265975026, 287.5298983642207986 ) ) ;
#10437 = CARTESIAN_POINT ( 'NONE',  ( 29.68009836720079875, 380.0000000000000000, -17.00000000000000355 ) ) ;
#10438 = CIRCLE ( 'NONE', #13195, 4.006599999998678108 ) ;
#10439 = CARTESIAN_POINT ( 'NONE',  ( -55.99999999999988631, 515.4878487013597805, -546.7230258972048205 ) ) ;
#10440 = FACE_OUTER_BOUND ( 'NONE', #4139, .T. ) ;
#10441 = DIRECTION ( 'NONE',  ( 0.000000000000000000, 0.000000000000000000, -1.000000000000000000 ) ) ;
#10442 = EDGE_CURVE ( 'NONE', #7330, #3010, #5241, .T. ) ;
#10443 = CARTESIAN_POINT ( 'NONE',  ( -55.99999999999989342, 473.6663340069157471, -531.5012393965008641 ) ) ;
#10444 = EDGE_CURVE ( 'NONE', #8527, #1812, #10252, .T. ) ;
#10445 = LINE ( 'NONE', #15433, #13166 ) ;
#10447 = VERTEX_POINT ( 'NONE', #9223 ) ;
#10446 = ORIENTED_EDGE ( 'NONE', *, *, #15997, .T. ) ;
#10448 = DIRECTION ( 'NONE',  ( 0.000000000000000000, 1.000000000000000000, 1.224646799147353207E-16 ) ) ;
#10449 = EDGE_CURVE ( 'NONE', #219, #12703, #7649, .T. ) ;
#10450 = ADVANCED_FACE ( 'NONE', ( #3640 ), #10336, .T. ) ;
#10451 = VECTOR ( 'NONE', #3386, 1000.000000000000000 ) ;
#10452 = ADVANCED_FACE ( 'NONE', ( #14118 ), #2339, .T. ) ;
#10453 = PLANE ( 'NONE',  #13500 ) ;
#10454 = EDGE_CURVE ( 'NONE', #4001, #204, #15823, .T. ) ;
#10455 = DIRECTION ( 'NONE',  ( 1.000000000000000000, 0.000000000000000000, 0.000000000000000000 ) ) ;
#10456 = DIRECTION ( 'NONE',  ( 1.000000000000000000, 0.000000000000000000, 0.000000000000000000 ) ) ;
#10457 = ORIENTED_EDGE ( 'NONE', *, *, #11377, .F. ) ;
#10458 = LINE ( 'NONE', #12699, #16792 ) ;
#10459 = DIRECTION ( 'NONE',  ( -0.000000000000000000, 1.000000000000000000, -0.000000000000000000 ) ) ;
#10460 = VERTEX_POINT ( 'NONE', #8358 ) ;
#10461 = DIRECTION ( 'NONE',  ( 0.000000000000000000, 0.000000000000000000, 1.000000000000000000 ) ) ;
#10462 = CARTESIAN_POINT ( 'NONE',  ( 45.00000000000000000, 515.4878487013597805, -546.7230258972048205 ) ) ;
#10463 = CARTESIAN_POINT ( 'NONE',  ( 44.68009836720079875, 352.3758082234937206, -75.00000000000000000 ) ) ;
#10464 = ORIENTED_EDGE ( 'NONE', *, *, #16425, .F. ) ;
#10465 = VECTOR ( 'NONE', #7909, 1000.000000000000000 ) ;
#10466 = DIRECTION ( 'NONE',  ( -3.854941057726255847E-16, -0.000000000000000000, 1.000000000000000000 ) ) ;
#10467 = DIRECTION ( 'NONE',  ( 0.000000000000000000, 1.000000000000000000, 1.224646799147353207E-16 ) ) ;
#10468 = VERTEX_POINT ( 'NONE', #3030 ) ;
#10469 = FACE_OUTER_BOUND ( 'NONE', #1401, .T. ) ;
#10470 = STYLED_ITEM ( 'NONE', ( #3574 ), #14111 ) ;
#10471 = CONTEXT_DEPENDENT_SHAPE_REPRESENTATION ( #9640, #3176 ) ;
#10472 = ADVANCED_FACE ( 'NONE', ( #5767, #1743, #3122, #10752, #16162, #15898 ), #14717, .T. ) ;
#10473 = CARTESIAN_POINT ( 'NONE',  ( 45.00000000000000000, 473.6663340069157471, -545.1966447803968094 ) ) ;
#10474 = AXIS2_PLACEMENT_3D ( 'NONE', #4043, #2924, #6691 ) ;
#10475 = EDGE_LOOP ( 'NONE', ( #14181, #15619, #8534, #12315 ) ) ;
#10476 = CARTESIAN_POINT ( 'NONE',  ( 26.00000000000001066, 68.00000000000000000, -31.00000000000002487 ) ) ;
#10477 = DIRECTION ( 'NONE',  ( 0.000000000000000000, 0.000000000000000000, -1.000000000000000000 ) ) ;
#10478 = CARTESIAN_POINT ( 'NONE',  ( 10.00000000000000000, 425.7506394335853201, 109.9999999999999858 ) ) ;
#10479 = VERTEX_POINT ( 'NONE', #1573 ) ;
#10480 = FACE_OUTER_BOUND ( 'NONE', #136, .T. ) ;
#10481 = CONICAL_SURFACE ( 'NONE', #10750, 12.64907335584850046, 0.003530080289784348537 ) ;
#10482 = CIRCLE ( 'NONE', #7720, 2.500000000000002220 ) ;
#10483 = DIRECTION ( 'NONE',  ( 0.000000000000000000, 0.000000000000000000, -1.000000000000000000 ) ) ;
#10484 = CYLINDRICAL_SURFACE ( 'NONE', #16614, 3.000000000000002665 ) ;
#10485 = EDGE_LOOP ( 'NONE', ( #12211, #4796, #2552, #6300 ) ) ;
#10486 = DIRECTION ( 'NONE',  ( 0.000000000000000000, 0.000000000000000000, 1.000000000000000000 ) ) ;
#10487 = ADVANCED_FACE ( 'NONE', ( #14801 ), #1831, .T. ) ;
#10488 = VERTEX_POINT ( 'NONE', #15989 ) ;
#10489 = ORIENTED_EDGE ( 'NONE', *, *, #3510, .F. ) ;
#10490 = DIRECTION ( 'NONE',  ( -0.000000000000000000, -0.000000000000000000, 1.000000000000000000 ) ) ;
#10491 = VERTEX_POINT ( 'NONE', #8179 ) ;
#10492 = CARTESIAN_POINT ( 'NONE',  ( 449.9999999999998295, 0.000000000000000000, -3.265806083553861003E-16 ) ) ;
#10493 = VECTOR ( 'NONE', #11484, 1000.000000000000000 ) ;
#10494 = VERTEX_POINT ( 'NONE', #6967 ) ;
#10495 = ORIENTED_EDGE ( 'NONE', *, *, #9088, .T. ) ;
#10496 = DIRECTION ( 'NONE',  ( 0.000000000000000000, -1.000000000000000000, 0.000000000000000000 ) ) ;
#10497 = DIRECTION ( 'NONE',  ( -0.000000000000000000, -1.000000000000000000, -0.000000000000000000 ) ) ;
#10498 =( REPRESENTATION_RELATIONSHIP ('NONE','NONE', #15822, #5843 ) REPRESENTATION_RELATIONSHIP_WITH_TRANSFORMATION ( #11677 )SHAPE_REPRESENTATION_RELATIONSHIP( ) );
#10499 = CIRCLE ( 'NONE', #16529, 2.999999999999995559 ) ;
#10500 = ORIENTED_EDGE ( 'NONE', *, *, #10667, .F. ) ;
#10501 = DIRECTION ( 'NONE',  ( 0.000000000000000000, 1.000000000000000000, 0.000000000000000000 ) ) ;
#10502 = CARTESIAN_POINT ( 'NONE',  ( 22.99999999999999645, 0.000000000000000000, 31.00000000000006750 ) ) ;
#10503 = AXIS2_PLACEMENT_3D ( 'NONE', #7659, #14039, #5169 ) ;
#10504 = FACE_BOUND ( 'NONE', #15252, .T. ) ;
#10505 = AXIS2_PLACEMENT_3D ( 'NONE', #15083, #15173, #7419 ) ;
#10506 = ORIENTED_EDGE ( 'NONE', *, *, #2887, .F. ) ;
#10507 = CARTESIAN_POINT ( 'NONE',  ( 55.99999999999989342, 473.6663340069158039, -561.9448123979092315 ) ) ;
#10508 = PLANE ( 'NONE',  #6931 ) ;
#10509 = VERTEX_POINT ( 'NONE', #542 ) ;
#10510 = DIRECTION ( 'NONE',  ( -1.000000000000000000, -0.000000000000000000, -0.000000000000000000 ) ) ;
#10511 = ORIENTED_EDGE ( 'NONE', *, *, #9623, .F. ) ;
#10512 = DIRECTION ( 'NONE',  ( -0.000000000000000000, -0.000000000000000000, 1.000000000000000000 ) ) ;
#10513 = VERTEX_POINT ( 'NONE', #461 ) ;
#10514 = PRESENTATION_LAYER_ASSIGNMENT (  '', '', ( #2571 ) ) ;
#10515 = ORIENTED_EDGE ( 'NONE', *, *, #13983, .T. ) ;
#10517 = LINE ( 'NONE', #9241, #4714 ) ;
#10516 = VECTOR ( 'NONE', #14485, 1000.000000000000000 ) ;
#10518 = VECTOR ( 'NONE', #16679, 1000.000000000000000 ) ;
#10519 = CARTESIAN_POINT ( 'NONE',  ( -20.99999999999999645, 8.000000000000000000, -35.00000000000000711 ) ) ;
#10520 = CARTESIAN_POINT ( 'NONE',  ( 25.99999999999997868, 8.000000000000000000, -39.99999999999999289 ) ) ;
#10521 = VERTEX_POINT ( 'NONE', #5506 ) ;
#10522 = EDGE_CURVE ( 'NONE', #7586, #2294, #2854, .T. ) ;
#10523 = CARTESIAN_POINT ( 'NONE',  ( -55.99999999999989342, 493.2350855268092573, -598.9613477082210693 ) ) ;
#10524 = VECTOR ( 'NONE', #10034, 1000.000000000000000 ) ;
#10525 = CARTESIAN_POINT ( 'NONE',  ( 394.0000000000001137, 341.5974953295075807, -105.4170192159777031 ) ) ;
#10526 = AXIS2_PLACEMENT_3D ( 'NONE', #16913, #7895, #15808 ) ;
#10527 = CARTESIAN_POINT ( 'NONE',  ( 46.99999999999988631, 549.5810598491749488, -575.3306267969850296 ) ) ;
#10528 = LINE ( 'NONE', #15765, #11442 ) ;
#10529 = DIRECTION ( 'NONE',  ( 0.000000000000000000, 0.000000000000000000, -1.000000000000000000 ) ) ;
#10530 = AXIS2_PLACEMENT_3D ( 'NONE', #13670, #1820, #704 ) ;
#10531 = EDGE_CURVE ( 'NONE', #12736, #6401, #13516, .T. ) ;
#10532 = DIRECTION ( 'NONE',  ( 1.000000000000000000, 0.000000000000000000, -0.000000000000000000 ) ) ;
#10533 = VECTOR ( 'NONE', #11873, 1000.000000000000000 ) ;
#10534 = DIRECTION ( 'NONE',  ( 0.000000000000000000, 0.000000000000000000, 1.000000000000000000 ) ) ;
#10536 = ORIENTED_EDGE ( 'NONE', *, *, #8529, .F. ) ;
#10535 = ORIENTED_EDGE ( 'NONE', *, *, #8917, .F. ) ;
#10537 = CARTESIAN_POINT ( 'NONE',  ( 2.980268877975829511, 40.60428768742846728, 9.020512128682495856 ) ) ;
#10538 = VECTOR ( 'NONE', #7156, 1000.000000000000000 ) ;
#10539 = CARTESIAN_POINT ( 'NONE',  ( -3.165718926339676109, 286.4868066975116676, 37.56780454546778714 ) ) ;
#10540 = CARTESIAN_POINT ( 'NONE',  ( 47.50000000000000000, 196.3050121726289206, 0.000000000000000000 ) ) ;
#10541 = DIRECTION ( 'NONE',  ( -1.000000000000000000, -0.000000000000000000, -0.000000000000000000 ) ) ;
#10542 = EDGE_LOOP ( 'NONE', ( #10270, #10683, #8093, #14715 ) ) ;
#10543 = ADVANCED_FACE ( 'NONE', ( #4140 ), #13254, .F. ) ;
#10544 = ADVANCED_FACE ( 'NONE', ( #13347 ), #4235, .T. ) ;
#10545 = AXIS2_PLACEMENT_3D ( 'NONE', #11947, #6775, #5483 ) ;
#10546 = FACE_OUTER_BOUND ( 'NONE', #16523, .T. ) ;
#10547 = PLANE ( 'NONE',  #8946 ) ;
#10548 = VERTEX_POINT ( 'NONE', #11966 ) ;
#10549 = FACE_OUTER_BOUND ( 'NONE', #12288, .T. ) ;
#10550 = VECTOR ( 'NONE', #1646, 1000.000000000000000 ) ;
#10551 = AXIS2_PLACEMENT_3D ( 'NONE', #11400, #14155, #10371 ) ;
#10552 = EDGE_CURVE ( 'NONE', #16161, #7717, #12128, .T. ) ;
#10553 = FACE_OUTER_BOUND ( 'NONE', #1590, .T. ) ;
#10554 = ORIENTED_EDGE ( 'NONE', *, *, #6958, .F. ) ;
#10555 = ADVANCED_FACE ( 'NONE', ( #2764 ), #14621, .T. ) ;
#10556 = ADVANCED_FACE ( 'NONE', ( #1651 ), #5687, .T. ) ;
#10557 = DIRECTION ( 'NONE',  ( 0.000000000000000000, 0.000000000000000000, -1.000000000000000000 ) ) ;
#10558 = DIRECTION ( 'NONE',  ( -0.000000000000000000, -1.000000000000000000, -0.000000000000000000 ) ) ;
#10559 = DIRECTION ( 'NONE',  ( 0.000000000000000000, 0.000000000000000000, 1.000000000000000000 ) ) ;
#10560 = ORIENTED_EDGE ( 'NONE', *, *, #13997, .T. ) ;
#10561 = CARTESIAN_POINT ( 'NONE',  ( 17.00000000000000000, 0.000000000000000000, -65.00000000000000000 ) ) ;
#10562 = CIRCLE ( 'NONE', #5334, 4.999999999999997335 ) ;
#10563 = DIRECTION ( 'NONE',  ( 1.000000000000000000, -3.400581542615706812E-15, 2.422066625794662531E-16 ) ) ;
#10564 = ORIENTED_EDGE ( 'NONE', *, *, #12600, .T. ) ;
#10565 = CARTESIAN_POINT ( 'NONE',  ( 46.99999999999988631, 523.2161522479888163, -507.5890438806159750 ) ) ;
#10566 = CARTESIAN_POINT ( 'NONE',  ( 46.99999999999988631, 473.6663340069158039, -561.9448123979092315 ) ) ;
#10567 = CARTESIAN_POINT ( 'NONE',  ( -37.00000000000000711, 10.00000000000000000, 23.00000000000000000 ) ) ;
#10568 = ORIENTED_EDGE ( 'NONE', *, *, #506, .T. ) ;
#10569 = LINE ( 'NONE', #6595, #2842 ) ;
#10570 = EDGE_CURVE ( 'NONE', #6355, #14833, #15404, .T. ) ;
#10571 = CARTESIAN_POINT ( 'NONE',  ( 46.99999999999988631, 559.9933750504617365, -546.7230258972048205 ) ) ;
#10572 = CARTESIAN_POINT ( 'NONE',  ( 3.000000000000000000, 1.836909530733570325E-16, 3.000000000000000000 ) ) ;
#10573 = ORIENTED_EDGE ( 'NONE', *, *, #6342, .F. ) ;
#10574 = EDGE_CURVE ( 'NONE', #15142, #6773, #10931, .T. ) ;
#10575 = AXIS2_PLACEMENT_3D ( 'NONE', #4437, #9852, #7083 ) ;
#10576 = EDGE_CURVE ( 'NONE', #8527, #9305, #7126, .T. ) ;
#10577 = ORIENTED_EDGE ( 'NONE', *, *, #5406, .F. ) ;
#10578 = ORIENTED_EDGE ( 'NONE', *, *, #6516, .F. ) ;
#10579 = CARTESIAN_POINT ( 'NONE',  ( -26.00000000000002132, 10.00000000000000000, -31.00000000000003553 ) ) ;
#10580 = EDGE_LOOP ( 'NONE', ( #479, #13268 ) ) ;
#10581 = EDGE_LOOP ( 'NONE', ( #3211, #1790, #3506, #10740 ) ) ;
#10582 = PRODUCT_CONTEXT ( 'NONE', #8297, 'mechanical' ) ;
#10583 = EDGE_LOOP ( 'NONE', ( #13734, #2087, #16689, #15407 ) ) ;
#10584 = ADVANCED_BREP_SHAPE_REPRESENTATION ( '', ( #14050, #1488 ), #16299 ) ;
#10585 = CIRCLE ( 'NONE', #3192, 4.695405383896011919 ) ;
#10586 = ORIENTED_EDGE ( 'NONE', *, *, #3922, .F. ) ;
#10587 = AXIS2_PLACEMENT_3D ( 'NONE', #220, #1244, #1327 ) ;
#10588 = DIRECTION ( 'NONE',  ( 0.000000000000000000, 0.000000000000000000, -1.000000000000000000 ) ) ;
#10589 = CARTESIAN_POINT ( 'NONE',  ( -26.00000000000002132, 10.00000000000000000, 40.00000000000000711 ) ) ;
#10590 = EDGE_LOOP ( 'NONE', ( #2823, #369, #9605, #15563 ) ) ;
#10591 = CARTESIAN_POINT ( 'NONE',  ( 36.99999999999999289, 10.00000000000000000, 17.99999999999998934 ) ) ;
#10592 = LINE ( 'NONE', #14541, #13643 ) ;
#10593 = ORIENTED_EDGE ( 'NONE', *, *, #14025, .T. ) ;
#10594 = FILL_AREA_STYLE_COLOUR ( '', #4745 ) ;
#10595 = VERTEX_POINT ( 'NONE', #16338 ) ;
#10596 = DIRECTION ( 'NONE',  ( 1.000000000000000000, 0.000000000000000000, 0.000000000000000000 ) ) ;
#10597 = FACE_OUTER_BOUND ( 'NONE', #12552, .T. ) ;
#10598 = VERTEX_POINT ( 'NONE', #11343 ) ;
#10599 = AXIS2_PLACEMENT_3D ( 'NONE', #6998, #2798, #2971 ) ;
#10600 = CIRCLE ( 'NONE', #8123, 4.000000000000007105 ) ;
#10601 = CARTESIAN_POINT ( 'NONE',  ( 0.000000000000000000, 66.00000000000000000, -5.741599279633704455E-16 ) ) ;
#10602 = ORIENTED_EDGE ( 'NONE', *, *, #15191, .T. ) ;
#10603 = FACE_BOUND ( 'NONE', #1484, .T. ) ;
#10604 = ORIENTED_EDGE ( 'NONE', *, *, #13151, .T. ) ;
#10605 = ORIENTED_EDGE ( 'NONE', *, *, #66, .T. ) ;
#10606 = CARTESIAN_POINT ( 'NONE',  ( -37.00000000000000711, 10.00000000000000000, -23.00000000000000000 ) ) ;
#10607 = EDGE_CURVE ( 'NONE', #14371, #1759, #10199, .T. ) ;
#10608 = DIRECTION ( 'NONE',  ( -1.000000000000000000, -0.000000000000000000, -0.000000000000000000 ) ) ;
#10609 = DIRECTION ( 'NONE',  ( 1.000000000000000000, 0.000000000000000000, 0.000000000000000000 ) ) ;
#10610 = VECTOR ( 'NONE', #15246, 1000.000000000000000 ) ;
#10611 = ORIENTED_EDGE ( 'NONE', *, *, #3426, .F. ) ;
#10612 = AXIS2_PLACEMENT_3D ( 'NONE', #11877, #15828, #8000 ) ;
#10613 = DIRECTION ( 'NONE',  ( -1.000000000000000000, -0.000000000000000000, -0.000000000000000000 ) ) ;
#10614 = DIRECTION ( 'NONE',  ( 0.000000000000000000, 0.000000000000000000, -1.000000000000000000 ) ) ;
#10615 = EDGE_CURVE ( 'NONE', #1299, #529, #11179, .T. ) ;
#10616 = DIRECTION ( 'NONE',  ( -1.000000000000000000, -0.000000000000000000, -0.000000000000000000 ) ) ;
#10617 = CARTESIAN_POINT ( 'NONE',  ( 46.99999999999988631, 473.6663340069158039, -561.9448123979092315 ) ) ;
#10618 = DIRECTION ( 'NONE',  ( -1.000000000000000000, 0.000000000000000000, 0.000000000000000000 ) ) ;
#10619 = DIRECTION ( 'NONE',  ( 0.000000000000000000, 1.000000000000000000, 0.000000000000000000 ) ) ;
#10621 = VERTEX_POINT ( 'NONE', #7460 ) ;
#10620 = VERTEX_POINT ( 'NONE', #15304 ) ;
#10622 = VECTOR ( 'NONE', #949, 1000.000000000000000 ) ;
#10623 = DIRECTION ( 'NONE',  ( 0.000000000000000000, 0.000000000000000000, 1.000000000000000000 ) ) ;
#10624 = PRODUCT_DEFINITION ( 'UNKNOWN', '', #5341, #15316 ) ;
#10625 = CARTESIAN_POINT ( 'NONE',  ( 0.05133912195941206513, 285.6265370167508877, 37.48177757739169635 ) ) ;
#10626 = DIRECTION ( 'NONE',  ( 0.000000000000000000, 0.000000000000000000, -1.000000000000000000 ) ) ;
#10627 = DIRECTION ( 'NONE',  ( 1.000000000000000000, 0.000000000000000000, 1.156482317317870344E-15 ) ) ;
#10628 = EDGE_CURVE ( 'NONE', #14978, #1977, #16587, .T. ) ;
#10629 = ORIENTED_EDGE ( 'NONE', *, *, #3634, .F. ) ;
#10630 = DIRECTION ( 'NONE',  ( 0.000000000000000000, 1.000000000000000000, 0.000000000000000000 ) ) ;
#10631 = MECHANICAL_DESIGN_GEOMETRIC_PRESENTATION_REPRESENTATION (  '', ( #5139 ), #8172 ) ;
#10632 = DIRECTION ( 'NONE',  ( 0.000000000000000000, -1.000000000000000000, 0.000000000000000000 ) ) ;
#10633 = VERTEX_POINT ( 'NONE', #3368 ) ;
#10634 = DIRECTION ( 'NONE',  ( 1.000000000000000000, 0.000000000000000000, -0.000000000000000000 ) ) ;
#10635 = LINE ( 'NONE', #13396, #13642 ) ;
#10636 = DIRECTION ( 'NONE',  ( 0.000000000000000000, 0.000000000000000000, 1.000000000000000000 ) ) ;
#10637 = DIRECTION ( 'NONE',  ( 0.000000000000000000, 0.000000000000000000, -1.000000000000000000 ) ) ;
#10638 = CARTESIAN_POINT ( 'NONE',  ( 0.3521046271551984685, 286.1171785048110792, 37.32951256787983851 ) ) ;
#10639 = ORIENTED_EDGE ( 'NONE', *, *, #900, .F. ) ;
#10640 = CARTESIAN_POINT ( 'NONE',  ( -46.99999999999988631, 473.6663340069158039, -561.9448123979092315 ) ) ;
#10641 = EDGE_CURVE ( 'NONE', #11540, #2523, #9893, .T. ) ;
#10642 = DIRECTION ( 'NONE',  ( 1.000000000000000000, 0.000000000000000000, 0.000000000000000000 ) ) ;
#10643 = AXIS2_PLACEMENT_3D ( 'NONE', #8248, #13496, #272 ) ;
#10644 = CARTESIAN_POINT ( 'NONE',  ( -2.220446049250313081E-13, 135.5000000000000000, 3.000000000000000000 ) ) ;
#10645 = ADVANCED_FACE ( 'NONE', ( #4816 ), #3283, .T. ) ;
#10646 = ORIENTED_EDGE ( 'NONE', *, *, #9515, .F. ) ;
#10647 = LINE ( 'NONE', #15967, #15964 ) ;
#10648 = UNCERTAINTY_MEASURE_WITH_UNIT (LENGTH_MEASURE( 1.000000000000000082E-05 ), #7623, 'distance_accuracy_value', 'NONE');
#10649 = DIRECTION ( 'NONE',  ( -0.000000000000000000, 1.000000000000000000, -0.000000000000000000 ) ) ;
#10650 = LINE ( 'NONE', #4705, #1005 ) ;
#10651 = VERTEX_POINT ( 'NONE', #15043 ) ;
#10652 = CARTESIAN_POINT ( 'NONE',  ( 45.00000000000000000, 559.9933750504617365, -546.7230258972048205 ) ) ;
#10653 = DIRECTION ( 'NONE',  ( -1.631319816340925608E-17, 0.000000000000000000, 1.000000000000000000 ) ) ;
#10654 = CARTESIAN_POINT ( 'NONE',  ( 37.00000000000000000, 68.00000000000000000, -23.00000000000000000 ) ) ;
#10655 = ORIENTED_EDGE ( 'NONE', *, *, #3324, .F. ) ;
#10656 = VECTOR ( 'NONE', #10212, 1000.000000000000000 ) ;
#10657 = ORIENTED_EDGE ( 'NONE', *, *, #7206, .F. ) ;
#10658 = EDGE_LOOP ( 'NONE', ( #12033, #9025 ) ) ;
#10659 = LINE ( 'NONE', #15982, #14110 ) ;
#10660 = EDGE_CURVE ( 'NONE', #3412, #614, #11559, .T. ) ;
#10661 = ADVANCED_FACE ( 'NONE', ( #8517 ), #5853, .T. ) ;
#10662 = EDGE_LOOP ( 'NONE', ( #3424, #4911, #10858, #10285 ) ) ;
#10663 = DIRECTION ( 'NONE',  ( 0.000000000000000000, 0.000000000000000000, 1.000000000000000000 ) ) ;
#10664 = VERTEX_POINT ( 'NONE', #12554 ) ;
#10665 = EDGE_CURVE ( 'NONE', #4071, #15905, #8441, .T. ) ;
#10666 = EDGE_CURVE ( 'NONE', #1685, #7040, #5532, .T. ) ;
#10667 = EDGE_CURVE ( 'NONE', #5865, #11589, #5940, .T. ) ;
#10668 = ORIENTED_EDGE ( 'NONE', *, *, #1760, .F. ) ;
#10669 = EDGE_CURVE ( 'NONE', #15569, #4216, #794, .T. ) ;
#10670 = CARTESIAN_POINT ( 'NONE',  ( -20.99999999999999645, 8.000000000000000000, 35.00000000000001421 ) ) ;
#10671 = CARTESIAN_POINT ( 'NONE',  ( -25.99999999999999645, 0.000000000000000000, 40.00000000000002132 ) ) ;
#10672 = VERTEX_POINT ( 'NONE', #2072 ) ;
#10673 = DIRECTION ( 'NONE',  ( 0.000000000000000000, 0.000000000000000000, 1.000000000000000000 ) ) ;
#10674 = DIRECTION ( 'NONE',  ( -1.000000000000000000, -0.000000000000000000, -0.000000000000000000 ) ) ;
#10675 = ORIENTED_EDGE ( 'NONE', *, *, #8399, .T. ) ;
#10676 = VECTOR ( 'NONE', #232, 1000.000000000000000 ) ;
#10677 = CARTESIAN_POINT ( 'NONE',  ( -37.00000000000000711, 10.00000000000000000, 23.00000000000000000 ) ) ;
#10678 = ORIENTED_EDGE ( 'NONE', *, *, #13174, .T. ) ;
#10679 = DIRECTION ( 'NONE',  ( 0.000000000000000000, 0.000000000000000000, -1.000000000000000000 ) ) ;
#10680 = LINE ( 'NONE', #5251, #1739 ) ;
#10681 = EDGE_LOOP ( 'NONE', ( #11847, #800, #9297, #11832 ) ) ;
#10682 = DIRECTION ( 'NONE',  ( 0.000000000000000000, 0.000000000000000000, 1.000000000000000000 ) ) ;
#10683 = ORIENTED_EDGE ( 'NONE', *, *, #696, .F. ) ;
#10684 =( NAMED_UNIT ( * ) SI_UNIT ( $, .STERADIAN. ) SOLID_ANGLE_UNIT ( ) );
#10685 = DIRECTION ( 'NONE',  ( 0.000000000000000000, 1.000000000000000000, 0.000000000000000000 ) ) ;
#10686 = EDGE_LOOP ( 'NONE', ( #11346, #7935 ) ) ;
#10687 = CIRCLE ( 'NONE', #8769, 1.800000000000000266 ) ;
#10688 = ORIENTED_EDGE ( 'NONE', *, *, #6073, .F. ) ;
#10689 = DIRECTION ( 'NONE',  ( -0.4740998230350218501, 0.8804710999221728729, 0.000000000000000000 ) ) ;
#10690 = ADVANCED_FACE ( 'NONE', ( #8608 ), #15121, .F. ) ;
#10691 = FACE_OUTER_BOUND ( 'NONE', #10187, .T. ) ;
#10692 = LINE ( 'NONE', #12246, #14362 ) ;
#10693 = ORIENTED_EDGE ( 'NONE', *, *, #13389, .F. ) ;
#10694 = LINE ( 'NONE', #10523, #12395 ) ;
#10695 = FACE_OUTER_BOUND ( 'NONE', #1054, .T. ) ;
#10696 = DIRECTION ( 'NONE',  ( 6.123031769111888756E-17, 0.000000000000000000, 1.000000000000000000 ) ) ;
#10697 = CARTESIAN_POINT ( 'NONE',  ( -45.00000000000000000, 515.4878487013597805, -546.7230258972048205 ) ) ;
#10698 = CYLINDRICAL_SURFACE ( 'NONE', #10769, 5.000000000000000888 ) ;
#10699 = VECTOR ( 'NONE', #2535, 1000.000000000000000 ) ;
#10700 = CARTESIAN_POINT ( 'NONE',  ( -40.00000000000000711, 10.00000000000000000, -19.00000000000000355 ) ) ;
#10701 = CARTESIAN_POINT ( 'NONE',  ( 0.000000000000000000, 372.8685141053783241, -146.8198051533979935 ) ) ;
#10702 = ADVANCED_FACE ( 'NONE', ( #11256 ), #11098, .F. ) ;
#10704 = ORIENTED_EDGE ( 'NONE', *, *, #7062, .F. ) ;
#10703 = EDGE_LOOP ( 'NONE', ( #11851, #9527, #4987, #2156 ) ) ;
#10705 = CARTESIAN_POINT ( 'NONE',  ( 3.000000000000000000, 41.00000000000000711, 9.013878188659973034 ) ) ;
#10706 = FACE_OUTER_BOUND ( 'NONE', #6241, .T. ) ;
#10707 = CARTESIAN_POINT ( 'NONE',  ( 75.00000000000000000, 380.0000000000000000, -7.000000000000006217 ) ) ;
#10708 = CARTESIAN_POINT ( 'NONE',  ( -23.00000000000000000, 0.000000000000000000, -36.99999999999999289 ) ) ;
#10709 = VECTOR ( 'NONE', #14439, 1000.000000000000000 ) ;
#10710 = EDGE_LOOP ( 'NONE', ( #3774, #2923, #2684, #15627 ) ) ;
#10711 = DIRECTION ( 'NONE',  ( 0.000000000000000000, 1.000000000000000000, -1.224646799147353207E-16 ) ) ;
#10712 = DIRECTION ( 'NONE',  ( 1.000000000000000000, -0.000000000000000000, 0.000000000000000000 ) ) ;
#10713 = VERTEX_POINT ( 'NONE', #6009 ) ;
#10714 = CARTESIAN_POINT ( 'NONE',  ( -26.00000000000000000, 19.00000000000000000, -31.00000000000003908 ) ) ;
#10715 = DIRECTION ( 'NONE',  ( 0.000000000000000000, 0.000000000000000000, 1.000000000000000000 ) ) ;
#10716 = DIRECTION ( 'NONE',  ( 0.000000000000000000, 0.000000000000000000, -1.000000000000000000 ) ) ;
#10717 = DIRECTION ( 'NONE',  ( -0.000000000000000000, -1.000000000000000000, -0.000000000000000000 ) ) ;
#10718 = DIRECTION ( 'NONE',  ( 1.000000000000000000, -0.000000000000000000, 0.000000000000000000 ) ) ;
#10719 = DIRECTION ( 'NONE',  ( -0.000000000000000000, -0.000000000000000000, -1.000000000000000000 ) ) ;
#10720 = ORIENTED_EDGE ( 'NONE', *, *, #13174, .F. ) ;
#10721 = DIRECTION ( 'NONE',  ( -1.000000000000000000, -0.000000000000000000, -0.000000000000000000 ) ) ;
#10722 = PRODUCT_DEFINITION_CONTEXT ( 'detailed design', #9180, 'design' ) ;
#10723 =( REPRESENTATION_RELATIONSHIP ('NONE','NONE', #15277, #16471 ) REPRESENTATION_RELATIONSHIP_WITH_TRANSFORMATION ( #3863 )SHAPE_REPRESENTATION_RELATIONSHIP( ) );
#10724 = DIRECTION ( 'NONE',  ( -1.000000000000000000, -0.000000000000000000, -0.000000000000000000 ) ) ;
#10725 = CARTESIAN_POINT ( 'NONE',  ( -46.99999999999988631, 523.2161522479893847, -590.5524132976893270 ) ) ;
#10726 = ORIENTED_EDGE ( 'NONE', *, *, #14985, .F. ) ;
#10727 = CARTESIAN_POINT ( 'NONE',  ( -55.99999999999988631, 460.1944820612779381, -191.6957561970704660 ) ) ;
#10728 = CARTESIAN_POINT ( 'NONE',  ( 0.000000000000000000, 425.7506394335853201, 305.2562418976663707 ) ) ;
#10729 = AXIS2_PLACEMENT_3D ( 'NONE', #15399, #8458, #3472 ) ;
#10730 = EDGE_CURVE ( 'NONE', #4486, #7744, #16250, .T. ) ;
#10731 = DIRECTION ( 'NONE',  ( 6.123031769111888756E-17, -1.000000000000000000, -3.749151804555344967E-33 ) ) ;
#10732 = VERTEX_POINT ( 'NONE', #8775 ) ;
#10733 = DIRECTION ( 'NONE',  ( 0.000000000000000000, 0.000000000000000000, -1.000000000000000000 ) ) ;
#10734 = CARTESIAN_POINT ( 'NONE',  ( -26.00000000000001776, 10.00000000000000000, 31.00000000000003553 ) ) ;
#10735 = CARTESIAN_POINT ( 'NONE',  ( 46.99999999999988631, 549.5810598491746077, -518.1154249974242703 ) ) ;
#10736 = VERTEX_POINT ( 'NONE', #4487 ) ;
#10737 = AXIS2_PLACEMENT_3D ( 'NONE', #9268, #16811, #1105 ) ;
#10738 = DIRECTION ( 'NONE',  ( 0.000000000000000000, 0.9271838545667884235, -0.3746065934159092947 ) ) ;
#10739 = AXIS2_PLACEMENT_3D ( 'NONE', #5196, #14067, #9173 ) ;
#10740 = ORIENTED_EDGE ( 'NONE', *, *, #14239, .T. ) ;
#10741 = ORIENTED_EDGE ( 'NONE', *, *, #10754, .F. ) ;
#10742 = EDGE_CURVE ( 'NONE', #12242, #7330, #9673, .T. ) ;
#10743 = CARTESIAN_POINT ( 'NONE',  ( 54.99999999999999289, 515.4878487013597805, -631.7230258972047068 ) ) ;
#10744 = ORIENTED_EDGE ( 'NONE', *, *, #11937, .T. ) ;
#10745 = DIRECTION ( 'NONE',  ( 1.000000000000000000, 0.000000000000000000, 0.000000000000000000 ) ) ;
#10746 = AXIS2_PLACEMENT_3D ( 'NONE', #1057, #8878, #12903 ) ;
#10747 = ORIENTED_EDGE ( 'NONE', *, *, #8416, .T. ) ;
#10748 = CIRCLE ( 'NONE', #2515, 12.00000000000000000 ) ;
#10749 = ORIENTED_EDGE ( 'NONE', *, *, #2149, .T. ) ;
#10750 = AXIS2_PLACEMENT_3D ( 'NONE', #10113, #5906, #16305 ) ;
#10751 = AXIS2_PLACEMENT_3D ( 'NONE', #10606, #13106, #14649 ) ;
#10752 = FACE_OUTER_BOUND ( 'NONE', #4935, .T. ) ;
#10753 = DIRECTION ( 'NONE',  ( -3.854941057726249437E-16, -0.000000000000000000, 1.000000000000000000 ) ) ;
#10754 = EDGE_CURVE ( 'NONE', #3722, #3171, #14346, .T. ) ;
#10755 = EDGE_LOOP ( 'NONE', ( #7080, #11029, #16347, #13204 ) ) ;
#10756 = LINE ( 'NONE', #6716, #10234 ) ;
#10757 = FACE_OUTER_BOUND ( 'NONE', #12463, .T. ) ;
#10758 = VERTEX_POINT ( 'NONE', #10476 ) ;
#10759 = VECTOR ( 'NONE', #15628, 1000.000000000000000 ) ;
#10760 = CARTESIAN_POINT ( 'NONE',  ( 40.00000000000000711, 0.000000000000000000, 34.99999999999997868 ) ) ;
#10761 = EDGE_CURVE ( 'NONE', #583, #16672, #16781, .T. ) ;
#10762 = ORIENTED_EDGE ( 'NONE', *, *, #16418, .T. ) ;
#10763 = FACE_BOUND ( 'NONE', #14312, .T. ) ;
#10764 = FACE_OUTER_BOUND ( 'NONE', #13945, .T. ) ;
#10765 = ORIENTED_EDGE ( 'NONE', *, *, #16211, .F. ) ;
#10766 = EDGE_CURVE ( 'NONE', #12146, #16177, #14095, .T. ) ;
#10767 = EDGE_CURVE ( 'NONE', #14326, #15448, #11507, .T. ) ;
#10768 = ADVANCED_FACE ( 'NONE', ( #8941 ), #6256, .T. ) ;
#10769 = AXIS2_PLACEMENT_3D ( 'NONE', #5541, #13547, #4176 ) ;
#10770 = VECTOR ( 'NONE', #7780, 1000.000000000000000 ) ;
#10771 = DIRECTION ( 'NONE',  ( -1.000000000000000000, -0.000000000000000000, -1.631319816340925608E-17 ) ) ;
#10772 = ORIENTED_EDGE ( 'NONE', *, *, #14412, .T. ) ;
#10773 = CARTESIAN_POINT ( 'NONE',  ( -31.00000000000001776, 10.00000000000000000, 31.00000000000000000 ) ) ;
#10774 = ORIENTED_EDGE ( 'NONE', *, *, #14213, .T. ) ;
#10775 = AXIS2_PLACEMENT_3D ( 'NONE', #14071, #14245, #9085 ) ;
#10776 = EDGE_LOOP ( 'NONE', ( #15253, #14816 ) ) ;
#10777 = CARTESIAN_POINT ( 'NONE',  ( -37.00000000000000711, 6.000000000000000000, -23.00000000000000000 ) ) ;
#10778 = CARTESIAN_POINT ( 'NONE',  ( 10.00000000000000000, 301.0487089519826327, 2.148629195649657075E-12 ) ) ;
#10779 = CARTESIAN_POINT ( 'NONE',  ( -34.99999999999998579, 3.000000000000000000, 23.50000000000000711 ) ) ;
#10780 = CARTESIAN_POINT ( 'NONE',  ( -430.0000000000000568, 425.7506394335853201, 109.9999999999999858 ) ) ;
#10781 = AXIS2_PLACEMENT_3D ( 'NONE', #14812, #2955, #2865 ) ;
#10782 = AXIS2_PLACEMENT_3D ( 'NONE', #5020, #11726, #10434 ) ;
#10783 = DIRECTION ( 'NONE',  ( 1.000000000000000000, 0.000000000000000000, 0.000000000000000000 ) ) ;
#10784 = CARTESIAN_POINT ( 'NONE',  ( -20.99999999999999645, 19.00000000000000000, -31.00000000000003908 ) ) ;
#10785 = DIRECTION ( 'NONE',  ( -0.000000000000000000, -1.000000000000000000, 0.000000000000000000 ) ) ;
#10786 = EDGE_CURVE ( 'NONE', #15233, #3412, #14436, .T. ) ;
#10787 = CARTESIAN_POINT ( 'NONE',  ( 1.050000000000000044, -15.25000000000000000, -1.867586368699713770E-15 ) ) ;
#10788 = LINE ( 'NONE', #2972, #1721 ) ;
#10789 = AXIS2_PLACEMENT_3D ( 'NONE', #6532, #7653, #7739 ) ;
#10790 = EDGE_CURVE ( 'NONE', #15586, #3442, #4898, .T. ) ;
#10791 = EDGE_CURVE ( 'NONE', #3447, #2369, #6422, .T. ) ;
#10792 = CARTESIAN_POINT ( 'NONE',  ( 39.06972645625037899, 346.7108172824755457, -6.736600000000000144 ) ) ;
#10793 = DIRECTION ( 'NONE',  ( 0.000000000000000000, 0.000000000000000000, 1.000000000000000000 ) ) ;
#10795 = VERTEX_POINT ( 'NONE', #11592 ) ;
#10794 = ORIENTED_EDGE ( 'NONE', *, *, #14231, .T. ) ;
#10796 = CARTESIAN_POINT ( 'NONE',  ( -3.270000000000000462, 289.4632308570086821, 37.52989836422091230 ) ) ;
#10797 = AXIS2_PLACEMENT_3D ( 'NONE', #6642, #11993, #10614 ) ;
#10798 = AXIS2_PLACEMENT_3D ( 'NONE', #9672, #4744, #15062 ) ;
#10799 = CARTESIAN_POINT ( 'NONE',  ( 1.286622718088548112E-12, 285.4366476906503749, 37.52989836422091940 ) ) ;
#10800 = DIRECTION ( 'NONE',  ( -0.000000000000000000, -1.000000000000000000, -0.000000000000000000 ) ) ;
#10801 = DIRECTION ( 'NONE',  ( 0.000000000000000000, 1.000000000000000000, -1.224646799147353207E-16 ) ) ;
#10802 = AXIS2_PLACEMENT_3D ( 'NONE', #14787, #15972, #8075 ) ;
#10803 = EDGE_LOOP ( 'NONE', ( #6698, #6469, #825, #16061 ) ) ;
#10804 = CARTESIAN_POINT ( 'NONE',  ( 10.00000000000000000, 381.0487089519837127, -150.0000000000032685 ) ) ;
#10805 = EDGE_CURVE ( 'NONE', #11864, #14282, #15554, .T. ) ;
#10806 = CARTESIAN_POINT ( 'NONE',  ( 10.00000000000000000, 364.9870314427752191, -206.3519347178565795 ) ) ;
#10807 = ORIENTED_EDGE ( 'NONE', *, *, #14550, .T. ) ;
#10808 = DIRECTION ( 'NONE',  ( 0.000000000000000000, 0.000000000000000000, 1.000000000000000000 ) ) ;
#10809 = CIRCLE ( 'NONE', #3406, 13.69540538389601991 ) ;
#10810 = CARTESIAN_POINT ( 'NONE',  ( 0.000000000000000000, 240.0523724647196389, -104.2090657433598011 ) ) ;
#10811 = CARTESIAN_POINT ( 'NONE',  ( 0.000000000000000000, 341.0487089519837696, -115.0000000000032969 ) ) ;
#10812 = VECTOR ( 'NONE', #13201, 1000.000000000000114 ) ;
#10813 = DIRECTION ( 'NONE',  ( 1.000000000000000000, 0.000000000000000000, 0.000000000000000000 ) ) ;
#10814 = FILL_AREA_STYLE_COLOUR ( '', #2683 ) ;
#10815 = FACE_OUTER_BOUND ( 'NONE', #12061, .T. ) ;
#10816 = ORIENTED_EDGE ( 'NONE', *, *, #16955, .T. ) ;
#10817 = CIRCLE ( 'NONE', #9997, 13.69540538389601991 ) ;
#10818 = DIRECTION ( 'NONE',  ( 1.000000000000000000, 0.000000000000000000, 0.000000000000000000 ) ) ;
#10819 = VECTOR ( 'NONE', #13152, 1000.000000000000000 ) ;
#10820 = PRODUCT_DEFINITION_FORMATION_WITH_SPECIFIED_SOURCE ( 'ANY', '', #7008, .NOT_KNOWN. ) ;
#10821 = DIRECTION ( 'NONE',  ( 0.000000000000000000, 0.000000000000000000, 1.000000000000000000 ) ) ;
#10822 = CIRCLE ( 'NONE', #13295, 4.695405383896011919 ) ;
#10823 = CARTESIAN_POINT ( 'NONE',  ( -23.00000000000002842, 0.000000000000000000, -31.00000000000003553 ) ) ;
#10824 = VERTEX_POINT ( 'NONE', #10227 ) ;
#10825 = ADVANCED_FACE ( 'NONE', ( #13143, #7807 ), #4, .T. ) ;
#10826 = PLANE ( 'NONE',  #14324 ) ;
#10827 = ADVANCED_FACE ( 'NONE', ( #9026 ), #7890, .T. ) ;
#10828 = DIRECTION ( 'NONE',  ( 0.000000000000000000, 0.000000000000000000, 1.000000000000000000 ) ) ;
#10829 = CARTESIAN_POINT ( 'NONE',  ( 25.99999999999998224, 10.00000000000000000, -31.00000000000003197 ) ) ;
#10830 = ORIENTED_EDGE ( 'NONE', *, *, #14412, .F. ) ;
#10831 = CARTESIAN_POINT ( 'NONE',  ( -45.00000000000000000, 549.5810598491749488, -575.3306267969850296 ) ) ;
#10832 = CARTESIAN_POINT ( 'NONE',  ( -31.81980515339462912, 0.000000000000000000, -35.11980515339465114 ) ) ;
#10833 = LINE ( 'NONE', #1724, #13885 ) ;
#10834 = ORIENTED_EDGE ( 'NONE', *, *, #8581, .T. ) ;
#10835 = EDGE_LOOP ( 'NONE', ( #16753, #16706, #1440, #2778 ) ) ;
#10836 = ORIENTED_EDGE ( 'NONE', *, *, #16531, .T. ) ;
#10837 = DIRECTION ( 'NONE',  ( -1.000000000000000000, 0.000000000000000000, 0.000000000000000000 ) ) ;
#10838 = AXIS2_PLACEMENT_3D ( 'NONE', #3699, #6251, #10220 ) ;
#10839 = ORIENTED_EDGE ( 'NONE', *, *, #16637, .F. ) ;
#10840 = PRODUCT_CONTEXT ( 'NONE', #5555, 'mechanical' ) ;
#10841 = EDGE_CURVE ( 'NONE', #4299, #15837, #5817, .T. ) ;
#10842 = PRODUCT_DEFINITION_SHAPE ( 'NONE', 'NONE',  #16974 ) ;
#10843 = ORIENTED_EDGE ( 'NONE', *, *, #14026, .T. ) ;
#10844 = ORIENTED_EDGE ( 'NONE', *, *, #264, .F. ) ;
#10845 = CARTESIAN_POINT ( 'NONE',  ( 35.00000000000000711, 19.00000000000000000, 20.99999999999999289 ) ) ;
#10846 = DIRECTION ( 'NONE',  ( -3.407805566942625851E-16, -0.09950371902099953980, -0.9950371902099891530 ) ) ;
#10847 = EDGE_CURVE ( 'NONE', #3545, #12955, #4183, .T. ) ;
#10848 = ORIENTED_EDGE ( 'NONE', *, *, #3573, .F. ) ;
#10849 = VECTOR ( 'NONE', #3405, 1000.000000000000000 ) ;
#10850 = DIRECTION ( 'NONE',  ( 0.000000000000000000, -0.000000000000000000, -1.000000000000000000 ) ) ;
#10851 = DIRECTION ( 'NONE',  ( -0.000000000000000000, -1.000000000000000000, -0.000000000000000000 ) ) ;
#10852 = ORIENTED_EDGE ( 'NONE', *, *, #540, .F. ) ;
#10853 = ORIENTED_EDGE ( 'NONE', *, *, #3116, .F. ) ;
#10854 = DIRECTION ( 'NONE',  ( 0.000000000000000000, 0.000000000000000000, 1.000000000000000000 ) ) ;
#10855 = FACE_OUTER_BOUND ( 'NONE', #12607, .T. ) ;
#10856 = EDGE_LOOP ( 'NONE', ( #4732, #13722, #3401, #10101 ) ) ;
#10857 = LINE ( 'NONE', #16095, #15372 ) ;
#10858 = ORIENTED_EDGE ( 'NONE', *, *, #12654, .T. ) ;
#10859 = CARTESIAN_POINT ( 'NONE',  ( 30.90550859392621064, -64.11391548236650806, 66.87703344121220539 ) ) ;
#10861 = CARTESIAN_POINT ( 'NONE',  ( -40.00000000000000000, 68.00000000000000000, 26.00000000000000355 ) ) ;
#10860 = VECTOR ( 'NONE', #16592, 1000.000000000000000 ) ;
#10862 = EDGE_CURVE ( 'NONE', #8711, #12822, #1290, .T. ) ;
#10863 = AXIS2_PLACEMENT_3D ( 'NONE', #10773, #6806, #13362 ) ;
#10864 = EDGE_CURVE ( 'NONE', #6790, #13878, #13522, .T. ) ;
#10865 = VERTEX_POINT ( 'NONE', #8855 ) ;
#10866 = VERTEX_POINT ( 'NONE', #7548 ) ;
#10867 = PRESENTATION_STYLE_ASSIGNMENT (( #13365 ) ) ;
#10868 = CARTESIAN_POINT ( 'NONE',  ( -46.99999999999988631, 473.6663340069158039, -566.6402177818052905 ) ) ;
#10869 = ADVANCED_FACE ( 'NONE', ( #12809 ), #16825, .F. ) ;
#10870 = DIRECTION ( 'NONE',  ( -0.000000000000000000, -1.000000000000000000, -0.000000000000000000 ) ) ;
#10871 = EDGE_CURVE ( 'NONE', #997, #12302, #13777, .T. ) ;
#10873 = ADVANCED_FACE ( 'NONE', ( #6853 ), #8070, .T. ) ;
#10872 = FACE_OUTER_BOUND ( 'NONE', #9667, .T. ) ;
#10874 = CYLINDRICAL_SURFACE ( 'NONE', #5860, 17.52499999999999858 ) ;
#10875 = AXIS2_PLACEMENT_3D ( 'NONE', #7197, #3269, #702 ) ;
#10876 = CARTESIAN_POINT ( 'NONE',  ( 32.99999999999998579, 10.00000000000000000, 25.99999999999999645 ) ) ;
#10877 = AXIS2_PLACEMENT_3D ( 'NONE', #14584, #78, #8052 ) ;
#10878 = FACE_OUTER_BOUND ( 'NONE', #16448, .T. ) ;
#10879 = DIRECTION ( 'NONE',  ( 1.000000000000000000, 0.000000000000000000, -0.000000000000000000 ) ) ;
#10880 = CARTESIAN_POINT ( 'NONE',  ( -45.00000000000000000, 523.2161522479888163, -489.1982331128240276 ) ) ;
#10881 = DIRECTION ( 'NONE',  ( -1.000000000000000000, -0.000000000000000000, -0.000000000000000000 ) ) ;
#10883 = ORIENTED_EDGE ( 'NONE', *, *, #11870, .F. ) ;
#10882 = EDGE_LOOP ( 'NONE', ( #14852, #11285, #4630, #16336 ) ) ;
#10884 = DIRECTION ( 'NONE',  ( 0.000000000000000000, -0.000000000000000000, 1.000000000000000000 ) ) ;
#10885 = EDGE_CURVE ( 'NONE', #5706, #14554, #14859, .T. ) ;
#10886 = AXIS2_PLACEMENT_3D ( 'NONE', #13375, #16111, #5451 ) ;
#10887 = DIRECTION ( 'NONE',  ( -1.000000000000000000, -0.000000000000000000, 0.000000000000000000 ) ) ;
#10888 = AXIS2_PLACEMENT_3D ( 'NONE', #13212, #9344, #13310 ) ;
#10889 = DIRECTION ( 'NONE',  ( -0.000000000000000000, 1.000000000000000000, -0.000000000000000000 ) ) ;
#10890 = EDGE_CURVE ( 'NONE', #614, #3412, #4720, .T. ) ;
#10891 = DIRECTION ( 'NONE',  ( -1.000000000000000000, 0.000000000000000000, 0.000000000000000000 ) ) ;
#10892 = ADVANCED_FACE ( 'NONE', ( #5402 ), #10913, .F. ) ;
#10894 = EDGE_LOOP ( 'NONE', ( #9466, #6863, #847, #554 ) ) ;
#10893 = EDGE_CURVE ( 'NONE', #16466, #11217, #10647, .T. ) ;
#10895 = ADVANCED_FACE ( 'NONE', ( #3007 ), #5578, .T. ) ;
#10896 = LINE ( 'NONE', #163, #10222 ) ;
#10897 = PLANE ( 'NONE',  #6739 ) ;
#10898 = VERTEX_POINT ( 'NONE', #10727 ) ;
#10899 = CARTESIAN_POINT ( 'NONE',  ( -46.99999999999988631, 473.6663340069157471, -531.5012393965008641 ) ) ;
#10900 = DIRECTION ( 'NONE',  ( 0.000000000000000000, 0.000000000000000000, 1.000000000000000000 ) ) ;
#10901 = CARTESIAN_POINT ( 'NONE',  ( -3.000000000000000000, 6.000000000000000000, 3.000000000000000000 ) ) ;
#10902 = CIRCLE ( 'NONE', #752, 13.69540538389601991 ) ;
#10903 = CIRCLE ( 'NONE', #8149, 4.999999999999997335 ) ;
#10904 = CARTESIAN_POINT ( 'NONE',  ( 449.9999999999998295, 135.5000000000000000, 0.000000000000000000 ) ) ;
#10905 = DIRECTION ( 'NONE',  ( 0.000000000000000000, 0.000000000000000000, 1.000000000000000000 ) ) ;
#10906 = CARTESIAN_POINT ( 'NONE',  ( -23.00000000000000000, 0.000000000000000000, -31.00000000000005684 ) ) ;
#10907 = ORIENTED_EDGE ( 'NONE', *, *, #14552, .T. ) ;
#10908 = CYLINDRICAL_SURFACE ( 'NONE', #11109, 13.69540538389601991 ) ;
#10909 = FACE_OUTER_BOUND ( 'NONE', #12542, .T. ) ;
#10910 = SURFACE_STYLE_USAGE ( .BOTH. , #1884 ) ;
#10911 = VECTOR ( 'NONE', #8845, 1000.000000000000000 ) ;
#10912 = ORIENTED_EDGE ( 'NONE', *, *, #281, .T. ) ;
#10913 = CYLINDRICAL_SURFACE ( 'NONE', #11846, 3.299999999999997158 ) ;
#10914 = CARTESIAN_POINT ( 'NONE',  ( -46.99999999999988631, 549.5810598491746077, -518.1154249974242703 ) ) ;
#10915 = EDGE_LOOP ( 'NONE', ( #16164, #804, #6977, #4826 ) ) ;
#10916 = DIRECTION ( 'NONE',  ( 1.000000000000000000, 0.000000000000000000, 0.000000000000000000 ) ) ;
#10917 = DIRECTION ( 'NONE',  ( -1.000000000000000000, 0.000000000000000000, 0.000000000000000000 ) ) ;
#10918 = DIRECTION ( 'NONE',  ( 0.000000000000000000, -0.3746065934159141242, 0.9271838545667866471 ) ) ;
#10919 = ORIENTED_EDGE ( 'NONE', *, *, #770, .F. ) ;
#10920 = CARTESIAN_POINT ( 'NONE',  ( 0.000000000000000000, 234.3157724647196289, -104.2090657433598011 ) ) ;
#10921 = ORIENTED_EDGE ( 'NONE', *, *, #16269, .T. ) ;
#10922 = ORIENTED_EDGE ( 'NONE', *, *, #13916, .T. ) ;
#10923 = AXIS2_PLACEMENT_3D ( 'NONE', #8576, #4617, #15188 ) ;
#10924 = DIRECTION ( 'NONE',  ( -0.000000000000000000, -1.000000000000000000, -0.000000000000000000 ) ) ;
#10925 = VECTOR ( 'NONE', #1852, 1000.000000000000000 ) ;
#10926 = ORIENTED_EDGE ( 'NONE', *, *, #801, .F. ) ;
#10927 = ADVANCED_FACE ( 'NONE', ( #4118 ), #10826, .T. ) ;
#10928 = ORIENTED_EDGE ( 'NONE', *, *, #241, .T. ) ;
#10929 = ADVANCED_FACE ( 'NONE', ( #16062 ), #4213, .F. ) ;
#10930 = EDGE_LOOP ( 'NONE', ( #11719, #2756, #2127, #6085 ) ) ;
#10931 = LINE ( 'NONE', #10670, #605 ) ;
#10932 = DIRECTION ( 'NONE',  ( 0.000000000000000000, 0.000000000000000000, 1.000000000000000000 ) ) ;
#10933 = ORIENTED_EDGE ( 'NONE', *, *, #8109, .F. ) ;
#10934 = CARTESIAN_POINT ( 'NONE',  ( 31.00000000000001421, 10.00000000000000000, 22.99999999999999645 ) ) ;
#10935 = APPLICATION_CONTEXT ( 'automotive_design' ) ;
#10936 = CARTESIAN_POINT ( 'NONE',  ( -31.00000000000005684, 10.00000000000000000, -23.00000000000000000 ) ) ;
#10937 = ORIENTED_EDGE ( 'NONE', *, *, #6894, .F. ) ;
#10938 = EDGE_CURVE ( 'NONE', #16590, #9423, #5546, .T. ) ;
#10939 = SURFACE_STYLE_USAGE ( .BOTH. , #126 ) ;
#10940 = EDGE_LOOP ( 'NONE', ( #11962, #15236 ) ) ;
#10941 = FACE_OUTER_BOUND ( 'NONE', #14349, .T. ) ;
#10942 = FACE_OUTER_BOUND ( 'NONE', #12912, .T. ) ;
#10943 = ORIENTED_EDGE ( 'NONE', *, *, #11478, .F. ) ;
#10944 = ORIENTED_EDGE ( 'NONE', *, *, #10730, .T. ) ;
#10945 = ADVANCED_FACE ( 'NONE', ( #15798 ), #14696, .T. ) ;
#10946 = CARTESIAN_POINT ( 'NONE',  ( 394.0000000000001137, 240.0523724647196389, -110.6822657433598067 ) ) ;
#10947 = VERTEX_POINT ( 'NONE', #8162 ) ;
#10948 = ORIENTED_EDGE ( 'NONE', *, *, #2792, .T. ) ;
#10949 = DIRECTION ( 'NONE',  ( -0.000000000000000000, -1.000000000000000000, -0.000000000000000000 ) ) ;
#10950 = DIRECTION ( 'NONE',  ( 0.000000000000000000, 0.000000000000000000, -1.000000000000000000 ) ) ;
#10951 = CARTESIAN_POINT ( 'NONE',  ( -31.00000000000000000, 19.00000000000000000, 30.99999999999999289 ) ) ;
#10952 = AXIS2_PLACEMENT_3D ( 'NONE', #15069, #12495, #9839 ) ;
#10953 = PLANE ( 'NONE',  #16505 ) ;
#10954 = CARTESIAN_POINT ( 'NONE',  ( 7.000000000000000000, 0.000000000000000000, 0.000000000000000000 ) ) ;
#10955 = EDGE_CURVE ( 'NONE', #11171, #1365, #1715, .T. ) ;
#10956 = CARTESIAN_POINT ( 'NONE',  ( -3.269999999997899476, 192.9646318551354227, 37.54886172132446376 ) ) ;
#10957 = FACE_OUTER_BOUND ( 'NONE', #8004, .T. ) ;
#10958 = CARTESIAN_POINT ( 'NONE',  ( 45.00000000000000000, 549.5810598491749488, -575.3306267969850296 ) ) ;
#10959 = DIRECTION ( 'NONE',  ( -1.000000000000000000, -0.000000000000000000, -0.000000000000000000 ) ) ;
#10960 = DIRECTION ( 'NONE',  ( 0.000000000000000000, 0.000000000000000000, -1.000000000000000000 ) ) ;
#10962 = ORIENTED_EDGE ( 'NONE', *, *, #10247, .F. ) ;
#10961 = VERTEX_POINT ( 'NONE', #9278 ) ;
#10963 = ADVANCED_FACE ( 'NONE', ( #4306 ), #14782, .F. ) ;
#10964 = CARTESIAN_POINT ( 'NONE',  ( 2.601523022692213694, 39.49322514888784497, 9.137549538570182150 ) ) ;
#10965 = AXIS2_PLACEMENT_3D ( 'NONE', #261, #10724, #14692 ) ;
#10966 = ADVANCED_FACE ( 'NONE', ( #12204 ), #13492, .T. ) ;
#10967 = SURFACE_STYLE_USAGE ( .BOTH. , #753 ) ;
#10968 = CARTESIAN_POINT ( 'NONE',  ( -31.00000000000006395, 0.000000000000000000, -25.99999999999999645 ) ) ;
#10969 = DIRECTION ( 'NONE',  ( -0.000000000000000000, -1.000000000000000000, -0.000000000000000000 ) ) ;
#10970 = ORIENTED_EDGE ( 'NONE', *, *, #2791, .T. ) ;
#10971 = COLOUR_RGB ( '', 0.08235294, 0.09019608, 0.10196078) ;
#10972 = DIRECTION ( 'NONE',  ( 1.000000000000000000, 0.000000000000000000, 0.000000000000000000 ) ) ;
#10974 = EDGE_CURVE ( 'NONE', #15231, #12156, #10208, .T. ) ;
#10973 = ORIENTED_EDGE ( 'NONE', *, *, #1855, .T. ) ;
#10975 = LINE ( 'NONE', #2033, #10976 ) ;
#10976 = VECTOR ( 'NONE', #4449, 1000.000000000000000 ) ;
#10977 = CARTESIAN_POINT ( 'NONE',  ( 54.99999999999999289, 515.4878487013597805, -546.7230258972048205 ) ) ;
#10978 = LINE ( 'NONE', #13569, #2796 ) ;
#10979 = AXIS2_PLACEMENT_3D ( 'NONE', #10305, #948, #3695 ) ;
#10980 = PRODUCT_DEFINITION_SHAPE ( 'NONE', 'NONE',  #14195 ) ;
#10981 = CARTESIAN_POINT ( 'NONE',  ( 10.00000000000000000, 306.0487089519837127, -150.0000000000038369 ) ) ;
#10982 =( NAMED_UNIT ( * ) PLANE_ANGLE_UNIT ( ) SI_UNIT ( $, .RADIAN. ) );
#10983 = ORIENTED_EDGE ( 'NONE', *, *, #9390, .F. ) ;
#10984 = EDGE_CURVE ( 'NONE', #9254, #1629, #4625, .T. ) ;
#10985 = EDGE_CURVE ( 'NONE', #5033, #1155, #3081, .T. ) ;
#10986 = EDGE_CURVE ( 'NONE', #8452, #1964, #1965, .T. ) ;
#10987 = CARTESIAN_POINT ( 'NONE',  ( 75.00000000000000000, 380.0000000000000000, 0.000000000000000000 ) ) ;
#10988 = EDGE_CURVE ( 'NONE', #7059, #13274, #1809, .T. ) ;
#10989 = VECTOR ( 'NONE', #6542, 1000.000000000000227 ) ;
#10990 = CARTESIAN_POINT ( 'NONE',  ( -26.00000000000000000, 19.00000000000000000, 40.00000000000001421 ) ) ;
#10991 = VECTOR ( 'NONE', #11282, 1000.000000000000000 ) ;
#10992 = LINE ( 'NONE', #262, #6918 ) ;
#10993 = ORIENTED_EDGE ( 'NONE', *, *, #11006, .T. ) ;
#10994 = DIRECTION ( 'NONE',  ( -0.000000000000000000, -0.000000000000000000, -1.000000000000000000 ) ) ;
#10995 = PRODUCT_DEFINITION_SHAPE ( 'NONE', 'NONE',  #9689 ) ;
#10996 = LINE ( 'NONE', #14785, #15793 ) ;
#10997 = ORIENTED_EDGE ( 'NONE', *, *, #3221, .T. ) ;
#10998 = DIRECTION ( 'NONE',  ( -1.000000000000000000, 3.424802208873653704E-15, 9.809413627650283915E-33 ) ) ;
#10999 = CYLINDRICAL_SURFACE ( 'NONE', #13408, 15.25000000000000000 ) ;
#11000 = FACE_OUTER_BOUND ( 'NONE', #8404, .T. ) ;
#11001 = ORIENTED_EDGE ( 'NONE', *, *, #2873, .F. ) ;
#11002 = AXIS2_PLACEMENT_3D ( 'NONE', #8771, #4022, #7455 ) ;
#11003 = ORIENTED_EDGE ( 'NONE', *, *, #4887, .T. ) ;
#11004 = EDGE_LOOP ( 'NONE', ( #7614, #13210 ) ) ;
#11005 = DIRECTION ( 'NONE',  ( -1.000000000000000000, -0.000000000000000000, -0.000000000000000000 ) ) ;
#11006 = EDGE_CURVE ( 'NONE', #2782, #12863, #7440, .T. ) ;
#11007 = VERTEX_POINT ( 'NONE', #13580 ) ;
#11008 = PRODUCT_CONTEXT ( 'NONE', #5664, 'mechanical' ) ;
#11009 = ORIENTED_EDGE ( 'NONE', *, *, #12318, .F. ) ;
#11010 = CARTESIAN_POINT ( 'NONE',  ( -33.00000000000000000, 10.00000000000000000, -26.00000000000000355 ) ) ;
#11011 = VECTOR ( 'NONE', #9322, 1000.000000000000227 ) ;
#11012 = EDGE_LOOP ( 'NONE', ( #12737, #5528, #12739, #4870 ) ) ;
#11013 = DIRECTION ( 'NONE',  ( -0.000000000000000000, -0.000000000000000000, 1.000000000000000000 ) ) ;
#11014 = CARTESIAN_POINT ( 'NONE',  ( 7.000000000000000000, 17.85000000000000142, 0.000000000000000000 ) ) ;
#11015 = ORIENTED_EDGE ( 'NONE', *, *, #8749, .T. ) ;
#11016 = FACE_OUTER_BOUND ( 'NONE', #8847, .T. ) ;
#11017 = DIRECTION ( 'NONE',  ( 0.000000000000000000, -0.9271838545667884235, 0.3746065934159092392 ) ) ;
#11018 = ORIENTED_EDGE ( 'NONE', *, *, #6044, .F. ) ;
#11019 = DIRECTION ( 'NONE',  ( 0.000000000000000000, 1.000000000000000000, 0.000000000000000000 ) ) ;
#11020 = ORIENTED_EDGE ( 'NONE', *, *, #8241, .T. ) ;
#11021 = CARTESIAN_POINT ( 'NONE',  ( 35.00000000000003553, -20.00000000000000000, -18.49999999999999645 ) ) ;
#11022 = ORIENTED_EDGE ( 'NONE', *, *, #12654, .F. ) ;
#11023 = AXIS2_PLACEMENT_3D ( 'NONE', #2945, #6712, #12047 ) ;
#11024 = ORIENTED_EDGE ( 'NONE', *, *, #10397, .F. ) ;
#11025 = DIRECTION ( 'NONE',  ( 1.000000000000000000, -1.476083657435421627E-31, -7.888609052210118054E-31 ) ) ;
#11026 = AXIS2_PLACEMENT_3D ( 'NONE', #4296, #8150, #10637 ) ;
#11027 = COLOUR_RGB ( '', 0.31764706, 0.68627451, 0.89019608) ;
#11028 = ORIENTED_EDGE ( 'NONE', *, *, #3845, .T. ) ;
#11029 = ORIENTED_EDGE ( 'NONE', *, *, #12840, .F. ) ;
#11030 = DIRECTION ( 'NONE',  ( 0.000000000000000000, 0.000000000000000000, -1.000000000000000000 ) ) ;
#11031 = CARTESIAN_POINT ( 'NONE',  ( 36.99999999999999289, 10.00000000000000000, 17.99999999999998934 ) ) ;
#11032 = CARTESIAN_POINT ( 'NONE',  ( 1.286622718088548112E-12, 285.4366476906530465, 37.52989836422116099 ) ) ;
#11033 = AXIS2_PLACEMENT_3D ( 'NONE', #182, #8330, #1372 ) ;
#11034 = CARTESIAN_POINT ( 'NONE',  ( 20.99999999999996092, 0.000000000000000000, 37.50000000000001421 ) ) ;
#11035 = CARTESIAN_POINT ( 'NONE',  ( -35.00000000000000000, 19.00000000000000000, -21.00000000000000000 ) ) ;
#11036 = CARTESIAN_POINT ( 'NONE',  ( 1.836909530733565148E-16, 0.000000000000000000, 3.000000000000000000 ) ) ;
#11037 = VECTOR ( 'NONE', #13114, 1000.000000000000000 ) ;
#11038 = CARTESIAN_POINT ( 'NONE',  ( 20.99999999999996092, -20.00000000000000000, 35.00000000000000711 ) ) ;
#11039 = AXIS2_PLACEMENT_3D ( 'NONE', #3958, #3865, #6688 ) ;
#11040 = EDGE_LOOP ( 'NONE', ( #14525, #13621, #6804, #6432 ) ) ;
#11041 = LINE ( 'NONE', #16282, #2107 ) ;
#11042 = CARTESIAN_POINT ( 'NONE',  ( -36.00000000000000711, 8.000000000000000000, -22.00000000000000355 ) ) ;
#11043 = CARTESIAN_POINT ( 'NONE',  ( 0.000000000000000000, 372.8685141053778693, -79.88019484660868841 ) ) ;
#11044 = LINE ( 'NONE', #12416, #15625 ) ;
#11046 = ORIENTED_EDGE ( 'NONE', *, *, #5912, .F. ) ;
#11045 = VERTEX_POINT ( 'NONE', #3347 ) ;
#11047 = CIRCLE ( 'NONE', #5260, 4.999999999999997335 ) ;
#11048 = CARTESIAN_POINT ( 'NONE',  ( 31.81980515339464333, 8.000000000000000000, -35.11980515339463693 ) ) ;
#11049 = ADVANCED_FACE ( 'NONE', ( #16473 ), #3515, .T. ) ;
#11050 = AXIS2_PLACEMENT_3D ( 'NONE', #11042, #13787, #4755 ) ;
#11051 = VECTOR ( 'NONE', #16314, 1000.000000000000000 ) ;
#11052 = DIRECTION ( 'NONE',  ( 0.000000000000000000, 0.000000000000000000, -1.000000000000000000 ) ) ;
#11053 = DIRECTION ( 'NONE',  ( 1.000000000000000000, 0.000000000000000000, 0.000000000000000000 ) ) ;
#11054 = ORIENTED_EDGE ( 'NONE', *, *, #11891, .F. ) ;
#11055 =( REPRESENTATION_RELATIONSHIP ('NONE','NONE', #9356, #11761 ) REPRESENTATION_RELATIONSHIP_WITH_TRANSFORMATION ( #1116 )SHAPE_REPRESENTATION_RELATIONSHIP( ) );
#11056 = AXIS2_PLACEMENT_3D ( 'NONE', #736, #6034, #1792 ) ;
#11057 = ADVANCED_FACE ( 'NONE', ( #6072 ), #6619, .T. ) ;
#11058 = DIRECTION ( 'NONE',  ( 0.000000000000000000, 0.000000000000000000, -1.000000000000000000 ) ) ;
#11059 = VERTEX_POINT ( 'NONE', #775 ) ;
#11060 = DIRECTION ( 'NONE',  ( 0.000000000000000000, 1.000000000000000000, 0.000000000000000000 ) ) ;
#11061 = CARTESIAN_POINT ( 'NONE',  ( 46.99999999999988631, 493.2350855268086320, -508.1801094700848580 ) ) ;
#11062 = LINE ( 'NONE', #3502, #13770 ) ;
#11063 = VECTOR ( 'NONE', #14784, 1000.000000000000000 ) ;
#11064 = LINE ( 'NONE', #4542, #8383 ) ;
#11065 = VECTOR ( 'NONE', #6751, 1000.000000000000000 ) ;
#11066 = FACE_OUTER_BOUND ( 'NONE', #5977, .T. ) ;
#11067 = ORIENTED_EDGE ( 'NONE', *, *, #2385, .F. ) ;
#11068 = CARTESIAN_POINT ( 'NONE',  ( 46.99999999999988631, 473.6663340069157471, -531.5012393965008641 ) ) ;
#11069 = VECTOR ( 'NONE', #12289, 1000.000000000000000 ) ;
#11070 = CARTESIAN_POINT ( 'NONE',  ( 31.00000000000001421, 10.00000000000000000, 25.99999999999999645 ) ) ;
#11071 = EDGE_CURVE ( 'NONE', #12856, #155, #13229, .T. ) ;
#11072 = PLANE ( 'NONE',  #1451 ) ;
#11073 = ORIENTED_EDGE ( 'NONE', *, *, #11609, .F. ) ;
#11074 = AXIS2_PLACEMENT_3D ( 'NONE', #9765, #15149, #9916 ) ;
#11075 = AXIS2_PLACEMENT_3D ( 'NONE', #12653, #9911, #16182 ) ;
#11076 = DIRECTION ( 'NONE',  ( -0.000000000000000000, -1.000000000000000000, -0.000000000000000000 ) ) ;
#11077 = ADVANCED_FACE ( 'NONE', ( #854 ), #5830, .T. ) ;
#11078 = ADVANCED_FACE ( 'NONE', ( #5991, #10045, #9716, #522, #7028, #14949 ), #8674, .T. ) ;
#11079 = DIRECTION ( 'NONE',  ( 0.000000000000000000, 1.000000000000000000, 0.000000000000000000 ) ) ;
#11080 = ORIENTED_EDGE ( 'NONE', *, *, #600, .F. ) ;
#11081 = DIRECTION ( 'NONE',  ( 1.000000000000000000, 0.000000000000000000, 0.000000000000000000 ) ) ;
#11082 = ADVANCED_FACE ( 'NONE', ( #11238 ), #13740, .F. ) ;
#11083 = DIRECTION ( 'NONE',  ( 1.000000000000000000, 0.000000000000000000, 0.000000000000000000 ) ) ;
#11084 = CARTESIAN_POINT ( 'NONE',  ( -3.000000000000002220, 60.00000000000000711, 6.000000000000000000 ) ) ;
#11085 = ORIENTED_EDGE ( 'NONE', *, *, #16958, .F. ) ;
#11086 = CIRCLE ( 'NONE', #3681, 60.00000000000002842 ) ;
#11087 =( LENGTH_UNIT ( ) NAMED_UNIT ( * ) SI_UNIT ( .MILLI., .METRE. ) );
#11088 = ORIENTED_EDGE ( 'NONE', *, *, #1659, .F. ) ;
#11089 = EDGE_LOOP ( 'NONE', ( #14027, #5009, #16946, #8190 ) ) ;
#11090 = VECTOR ( 'NONE', #7038, 1000.000000000000000 ) ;
#11091 = CARTESIAN_POINT ( 'NONE',  ( 54.99999999999999289, 515.4878487013597805, -359.2230258972048773 ) ) ;
#11092 = CIRCLE ( 'NONE', #9164, 187.4999999999998863 ) ;
#11093 = VECTOR ( 'NONE', #10497, 1000.000000000000000 ) ;
#11094 = ITEM_DEFINED_TRANSFORMATION ( 'NONE', 'NONE', #11362,  #1488 ) ;
#11095 = VECTOR ( 'NONE', #1732, 1000.000000000000000 ) ;
#11096 = LINE ( 'NONE', #11177, #4104 ) ;
#11097 = VERTEX_POINT ( 'NONE', #12610 ) ;
#11098 = CYLINDRICAL_SURFACE ( 'NONE', #7175, 3.000000000000000000 ) ;
#11099 = EDGE_CURVE ( 'NONE', #8068, #7931, #13662, .T. ) ;
#11100 = DIRECTION ( 'NONE',  ( -2.922523701604180730E-15, 0.9950371902099879318, 0.09950371902101125265 ) ) ;
#11101 = EDGE_CURVE ( 'NONE', #10468, #13251, #16318, .T. ) ;
#11102 = AXIS2_PLACEMENT_3D ( 'NONE', #15893, #13597, #8089 ) ;
#11103 = EDGE_LOOP ( 'NONE', ( #7836, #6519 ) ) ;
#11104 = DIRECTION ( 'NONE',  ( 0.000000000000000000, 0.000000000000000000, 1.000000000000000000 ) ) ;
#11105 = EDGE_CURVE ( 'NONE', #8468, #13435, #3263, .T. ) ;
#11106 = CIRCLE ( 'NONE', #10287, 0.7366000000000004766 ) ;
#11107 = DIRECTION ( 'NONE',  ( 1.000000000000000000, 0.000000000000000000, 0.000000000000000000 ) ) ;
#11108 = EDGE_LOOP ( 'NONE', ( #14959, #14493, #1147, #4677 ) ) ;
#11109 = AXIS2_PLACEMENT_3D ( 'NONE', #8230, #6845, #177 ) ;
#11110 = AXIS2_PLACEMENT_3D ( 'NONE', #4868, #6305, #3589 ) ;
#11111 = ORIENTED_EDGE ( 'NONE', *, *, #16916, .T. ) ;
#11112 = ORIENTED_EDGE ( 'NONE', *, *, #5524, .T. ) ;
#11113 = ORIENTED_EDGE ( 'NONE', *, *, #9875, .T. ) ;
#11114 =( LENGTH_UNIT ( ) NAMED_UNIT ( * ) SI_UNIT ( .MILLI., .METRE. ) );
#11115 = ORIENTED_EDGE ( 'NONE', *, *, #16093, .F. ) ;
#11116 = VERTEX_POINT ( 'NONE', #692 ) ;
#11117 = CARTESIAN_POINT ( 'NONE',  ( 394.0000000000001137, 240.0523724647196389, -17.15546574335979813 ) ) ;
#11118 = AXIS2_PLACEMENT_3D ( 'NONE', #1867, #16450, #4676 ) ;
#11119 = DIRECTION ( 'NONE',  ( 0.000000000000000000, 0.000000000000000000, -1.000000000000000000 ) ) ;
#11120 = CARTESIAN_POINT ( 'NONE',  ( 31.00000000000003553, 19.00000000000000000, 20.99999999999999289 ) ) ;
#11121 = LINE ( 'NONE', #9501, #10925 ) ;
#11122 = DIRECTION ( 'NONE',  ( 0.000000000000000000, 0.000000000000000000, -1.000000000000000000 ) ) ;
#11123 = DIRECTION ( 'NONE',  ( 0.000000000000000000, 1.000000000000000000, 0.000000000000000000 ) ) ;
#11124 = DIRECTION ( 'NONE',  ( 0.000000000000000000, 1.000000000000000000, -9.899245676326632924E-17 ) ) ;
#11125 = ORIENTED_EDGE ( 'NONE', *, *, #15988, .F. ) ;
#11126 = DIRECTION ( 'NONE',  ( 0.000000000000000000, 0.000000000000000000, -1.000000000000000000 ) ) ;
#11127 = CARTESIAN_POINT ( 'NONE',  ( -46.99999999999988631, 523.2161522479888163, -516.5890438806160319 ) ) ;
#11128 = AXIS2_PLACEMENT_3D ( 'NONE', #827, #6049, #4852 ) ;
#11129 = DIRECTION ( 'NONE',  ( 0.000000000000000000, 0.000000000000000000, -1.000000000000000000 ) ) ;
#11130 = CARTESIAN_POINT ( 'NONE',  ( -26.00000000000002132, 10.00000000000000000, -31.00000000000003553 ) ) ;
#11132 = ORIENTED_EDGE ( 'NONE', *, *, #9381, .F. ) ;
#11131 = ORIENTED_EDGE ( 'NONE', *, *, #4464, .T. ) ;
#11133 = CARTESIAN_POINT ( 'NONE',  ( 35.99999999999999289, 8.000000000000000000, 18.99999999999999289 ) ) ;
#11134 = EDGE_LOOP ( 'NONE', ( #10425, #2947 ) ) ;
#11135 = ADVANCED_FACE ( 'NONE', ( #16396 ), #9755, .F. ) ;
#11136 = FILL_AREA_STYLE ('',( #5974 ) ) ;
#11137 = LINE ( 'NONE', #14051, #3045 ) ;
#11138 = CARTESIAN_POINT ( 'NONE',  ( -35.00000000000000000, 19.00000000000000000, 20.99999999999999289 ) ) ;
#11139 = VECTOR ( 'NONE', #15032, 1000.000000000000000 ) ;
#11140 = ORIENTED_EDGE ( 'NONE', *, *, #11360, .T. ) ;
#11141 = EDGE_CURVE ( 'NONE', #10824, #7385, #10499, .T. ) ;
#11142 = CIRCLE ( 'NONE', #10888, 4.999999999999997335 ) ;
#11143 = CARTESIAN_POINT ( 'NONE',  ( 0.000000000000000000, 339.1725919290084335, -104.9456657433597968 ) ) ;
#11144 = CARTESIAN_POINT ( 'NONE',  ( 3.500000000000000000, 0.000000000000000000, 0.000000000000000000 ) ) ;
#11145 = EDGE_LOOP ( 'NONE', ( #1990, #15336, #6878, #8210 ) ) ;
#11146 = CARTESIAN_POINT ( 'NONE',  ( -3.000000000000003109, 60.00000000000000711, 9.013878188659973034 ) ) ;
#11147 = DIRECTION ( 'NONE',  ( 0.000000000000000000, 0.000000000000000000, -1.000000000000000000 ) ) ;
#11148 = DIRECTION ( 'NONE',  ( 0.000000000000000000, 0.000000000000000000, 1.000000000000000000 ) ) ;
#11149 = DIRECTION ( 'NONE',  ( -0.000000000000000000, -1.000000000000000000, -0.000000000000000000 ) ) ;
#11150 = DIRECTION ( 'NONE',  ( 0.000000000000000000, -1.000000000000000000, 0.000000000000000000 ) ) ;
#11151 = ORIENTED_EDGE ( 'NONE', *, *, #4684, .F. ) ;
#11152 = AXIS2_PLACEMENT_3D ( 'NONE', #3253, #7173, #843 ) ;
#11153 = CARTESIAN_POINT ( 'NONE',  ( -31.81980515339462912, 0.000000000000000000, -31.81980515339465043 ) ) ;
#11154 = AXIS2_PLACEMENT_3D ( 'NONE', #164, #2813, #5465 ) ;
#11155 = ADVANCED_FACE ( 'NONE', ( #4954 ), #13792, .T. ) ;
#11156 = CYLINDRICAL_SURFACE ( 'NONE', #13439, 3.300000000000025135 ) ;
#11157 = ORIENTED_EDGE ( 'NONE', *, *, #14552, .F. ) ;
#11158 = APPLICATION_CONTEXT ( 'automotive_design' ) ;
#11159 = LINE ( 'NONE', #8832, #2532 ) ;
#11160 = ORIENTED_EDGE ( 'NONE', *, *, #12244, .T. ) ;
#11161 = CARTESIAN_POINT ( 'NONE',  ( 29.68009836720079875, 352.3758082234937206, -75.00000000000000000 ) ) ;
#11162 = CIRCLE ( 'NONE', #14466, 13.69540538389598083 ) ;
#11163 = FACE_BOUND ( 'NONE', #11490, .T. ) ;
#11164 = VERTEX_POINT ( 'NONE', #11661 ) ;
#11165 = AXIS2_PLACEMENT_3D ( 'NONE', #15633, #9209, #14444 ) ;
#11166 = LINE ( 'NONE', #7787, #6397 ) ;
#11167 = DIRECTION ( 'NONE',  ( 0.000000000000000000, 0.000000000000000000, -1.000000000000000000 ) ) ;
#11168 = CARTESIAN_POINT ( 'NONE',  ( 56.73000000000001108, 239.4632308570078294, 71.73739990498292229 ) ) ;
#11169 = EDGE_LOOP ( 'NONE', ( #3407, #438, #6824, #12369 ) ) ;
#11170 = EDGE_CURVE ( 'NONE', #3203, #13507, #3597, .T. ) ;
#11171 = VERTEX_POINT ( 'NONE', #10207 ) ;
#11172 = EDGE_LOOP ( 'NONE', ( #457, #467, #5544, #11522, #4960, #1894, #14760, #12479, #5079, #5374, #6365, #11254, #3222, #3693, #3838, #11653 ) ) ;
#11173 = FACE_OUTER_BOUND ( 'NONE', #13339, .T. ) ;
#11174 = APPLICATION_PROTOCOL_DEFINITION ( 'draft international standard', 'automotive_design', 1998, #2371 ) ;
#11175 = AXIS2_PLACEMENT_3D ( 'NONE', #9485, #6801, #3993 ) ;
#11176 = EDGE_CURVE ( 'NONE', #5863, #10865, #11585, .T. ) ;
#11177 = CARTESIAN_POINT ( 'NONE',  ( 17.00000000000000711, 380.0000000000000000, -17.00000000000000355 ) ) ;
#11178 = ORIENTED_EDGE ( 'NONE', *, *, #782, .F. ) ;
#11179 = LINE ( 'NONE', #14970, #12393 ) ;
#11180 = CYLINDRICAL_SURFACE ( 'NONE', #5873, 3.300000000000025135 ) ;
#11181 = ORIENTED_EDGE ( 'NONE', *, *, #3706, .F. ) ;
#11182 = DIRECTION ( 'NONE',  ( -0.000000000000000000, -1.000000000000000000, 0.000000000000000000 ) ) ;
#11183 = CARTESIAN_POINT ( 'NONE',  ( 1.232007831292310690E-12, 193.4898140233672450, 37.52989836422092651 ) ) ;
#11184 = ORIENTED_EDGE ( 'NONE', *, *, #8562, .T. ) ;
#11185 = CIRCLE ( 'NONE', #3784, 5.000000000000004441 ) ;
#11186 = ADVANCED_FACE ( 'NONE', ( #7439 ), #2812, .F. ) ;
#11187 = LINE ( 'NONE', #16421, #12998 ) ;
#11188 = ORIENTED_EDGE ( 'NONE', *, *, #3510, .T. ) ;
#11189 = EDGE_LOOP ( 'NONE', ( #14593, #7390 ) ) ;
#11190 = EDGE_LOOP ( 'NONE', ( #14357, #14969, #4258, #16918 ) ) ;
#11191 = EDGE_CURVE ( 'NONE', #13435, #16667, #10458, .T. ) ;
#11192 = EDGE_CURVE ( 'NONE', #11248, #7717, #1098, .T. ) ;
#11193 = EDGE_CURVE ( 'NONE', #4052, #5619, #15162, .T. ) ;
#11194 = ADVANCED_FACE ( 'NONE', ( #12789 ), #8834, .F. ) ;
#11195 = EDGE_LOOP ( 'NONE', ( #16072, #7391, #16126, #6024 ) ) ;
#11196 = EDGE_LOOP ( 'NONE', ( #6158, #6079, #2810, #12471 ) ) ;
#11197 = CARTESIAN_POINT ( 'NONE',  ( -2.383085342081997293, 39.16728066132458963, 9.196931476227280911 ) ) ;
#11198 = AXIS2_PLACEMENT_3D ( 'NONE', #7146, #13626, #12072 ) ;
#11199 = CARTESIAN_POINT ( 'NONE',  ( 31.81980515339464333, 11.00000000000000000, 31.81980515339463622 ) ) ;
#11200 = DIRECTION ( 'NONE',  ( 0.01502673813723916056, -0.9998870921963913805, 0.000000000000000000 ) ) ;
#11201 = LINE ( 'NONE', #3389, #8183 ) ;
#11202 = DIRECTION ( 'NONE',  ( -0.000000000000000000, 0.000000000000000000, -1.000000000000000000 ) ) ;
#11203 = DIRECTION ( 'NONE',  ( 0.000000000000000000, 0.000000000000000000, 1.000000000000000000 ) ) ;
#11204 = CYLINDRICAL_SURFACE ( 'NONE', #11800, 3.000000000000000000 ) ;
#11205 = LINE ( 'NONE', #12579, #7093 ) ;
#11206 = ORIENTED_EDGE ( 'NONE', *, *, #15895, .T. ) ;
#11207 = DIRECTION ( 'NONE',  ( 0.000000000000000000, 0.000000000000000000, -1.000000000000000000 ) ) ;
#11208 = CARTESIAN_POINT ( 'NONE',  ( 21.00000000000000000, 8.000000000000000000, 31.00000000000006395 ) ) ;
#11209 = PLANE ( 'NONE',  #6963 ) ;
#11210 = VECTOR ( 'NONE', #6996, 1000.000000000000000 ) ;
#11211 = SHAPE_REPRESENTATION ( 'Servo-Head', ( #1488 ), #15199 ) ;
#11212 = CARTESIAN_POINT ( 'NONE',  ( -40.00000000000000711, 10.00000000000000000, 26.00000000000000000 ) ) ;
#11214 = ORIENTED_EDGE ( 'NONE', *, *, #8787, .T. ) ;
#11213 = ORIENTED_EDGE ( 'NONE', *, *, #6032, .F. ) ;
#11215 = PLANE ( 'NONE',  #11118 ) ;
#11216 = EDGE_CURVE ( 'NONE', #4234, #10468, #11047, .T. ) ;
#11217 = VERTEX_POINT ( 'NONE', #12864 ) ;
#11218 = SURFACE_SIDE_STYLE ('',( #13716 ) ) ;
#11219 = DIRECTION ( 'NONE',  ( 1.000000000000000000, 0.000000000000000000, 0.000000000000000000 ) ) ;
#11220 = DIRECTION ( 'NONE',  ( 1.000000000000000000, -0.000000000000000000, -0.000000000000000000 ) ) ;
#11221 = ORIENTED_EDGE ( 'NONE', *, *, #1107, .F. ) ;
#11222 = PRODUCT_DEFINITION_CONTEXT ( 'detailed design', #2147, 'design' ) ;
#11223 = CARTESIAN_POINT ( 'NONE',  ( 10.00000000000000000, 309.2289037985890445, -146.8198051533984199 ) ) ;
#11224 = DIRECTION ( 'NONE',  ( 0.000000000000000000, 0.000000000000000000, 1.000000000000000000 ) ) ;
#11225 = ORIENTED_EDGE ( 'NONE', *, *, #13099, .T. ) ;
#11226 = CARTESIAN_POINT ( 'NONE',  ( 1.163414457778310218E-15, 63.00000000000000000, 9.500000000000000000 ) ) ;
#11227 = CARTESIAN_POINT ( 'NONE',  ( 45.00000000000000000, 515.4878487013597805, -546.7230258972048205 ) ) ;
#11228 = DIRECTION ( 'NONE',  ( 0.000000000000000000, 0.000000000000000000, 1.000000000000000000 ) ) ;
#11229 = FACE_OUTER_BOUND ( 'NONE', #12068, .T. ) ;
#11230 = DIRECTION ( 'NONE',  ( -0.000000000000000000, 1.000000000000000000, -0.000000000000000000 ) ) ;
#11231 = ORIENTED_EDGE ( 'NONE', *, *, #2477, .T. ) ;
#11232 = DIRECTION ( 'NONE',  ( 1.000000000000000000, 0.000000000000000000, 0.000000000000000000 ) ) ;
#11233 = DIRECTION ( 'NONE',  ( 1.000000000000000000, 0.000000000000000000, 0.000000000000000000 ) ) ;
#11234 = EDGE_LOOP ( 'NONE', ( #7662, #1892, #4778, #16560, #24 ) ) ;
#11235 = LINE ( 'NONE', #7187, #2820 ) ;
#11236 = VECTOR ( 'NONE', #10881, 1000.000000000000000 ) ;
#11237 = VERTEX_POINT ( 'NONE', #15535 ) ;
#11238 = FACE_OUTER_BOUND ( 'NONE', #7398, .T. ) ;
#11239 = CARTESIAN_POINT ( 'NONE',  ( 1.347066989204613998E-15, -1.203706215242022682E-32, 24.99999999999999645 ) ) ;
#11240 = ORIENTED_EDGE ( 'NONE', *, *, #9937, .T. ) ;
#11241 = CARTESIAN_POINT ( 'NONE',  ( -46.99999999999988631, 549.5810598491746077, -504.4200196135282113 ) ) ;
#11242 = CARTESIAN_POINT ( 'NONE',  ( 0.000000000000000000, 341.4647406485092915, -16.00114864346762644 ) ) ;
#11243 = CARTESIAN_POINT ( 'NONE',  ( -20.99999999999999645, 19.00000000000000000, -35.00000000000000711 ) ) ;
#11244 = ORIENTED_EDGE ( 'NONE', *, *, #12414, .T. ) ;
#11245 = DIRECTION ( 'NONE',  ( 0.000000000000000000, -1.000000000000000000, 0.000000000000000000 ) ) ;
#11246 = SURFACE_STYLE_FILL_AREA ( #14890 ) ;
#11247 = EDGE_LOOP ( 'NONE', ( #4643, #9570, #6551, #3370 ) ) ;
#11248 = VERTEX_POINT ( 'NONE', #4878 ) ;
#11249 = CARTESIAN_POINT ( 'NONE',  ( 0.000000000000000000, -3.000000000000000000, 0.000000000000000000 ) ) ;
#11250 = AXIS2_PLACEMENT_3D ( 'NONE', #7264, #16460, #3332 ) ;
#11251 = SHAPE_DEFINITION_REPRESENTATION ( #13611, #8805 ) ;
#11252 =( NAMED_UNIT ( * ) SI_UNIT ( $, .STERADIAN. ) SOLID_ANGLE_UNIT ( ) );
#11253 = CARTESIAN_POINT ( 'NONE',  ( 1.983673311716144694, 62.25902922769662240, 9.291669371308648451 ) ) ;
#11254 = ORIENTED_EDGE ( 'NONE', *, *, #10522, .F. ) ;
#11255 = EDGE_CURVE ( 'NONE', #12055, #14343, #9400, .T. ) ;
#11256 = FACE_OUTER_BOUND ( 'NONE', #7047, .T. ) ;
#11257 = CYLINDRICAL_SURFACE ( 'NONE', #8630, 12.00000000000000178 ) ;
#11258 = AXIS2_PLACEMENT_3D ( 'NONE', #9175, #5381, #2720 ) ;
#11259 = ORIENTED_EDGE ( 'NONE', *, *, #16229, .T. ) ;
#11260 = CARTESIAN_POINT ( 'NONE',  ( 1.224646799147347044E-16, 38.00000000000000711, -0.9999999999999956701 ) ) ;
#11261 = DIRECTION ( 'NONE',  ( -0.000000000000000000, -0.000000000000000000, 1.000000000000000000 ) ) ;
#11262 = ORIENTED_EDGE ( 'NONE', *, *, #6250, .T. ) ;
#11263 = EDGE_CURVE ( 'NONE', #2294, #15644, #3771, .T. ) ;
#11264 = DIRECTION ( 'NONE',  ( 0.000000000000000000, 0.000000000000000000, 1.000000000000000000 ) ) ;
#11265 = ORIENTED_EDGE ( 'NONE', *, *, #16562, .T. ) ;
#11266 = ORIENTED_EDGE ( 'NONE', *, *, #5311, .F. ) ;
#11267 = ORIENTED_EDGE ( 'NONE', *, *, #7918, .T. ) ;
#11268 =( NAMED_UNIT ( * ) PLANE_ANGLE_UNIT ( ) SI_UNIT ( $, .RADIAN. ) );
#11269 = CIRCLE ( 'NONE', #849, 14.76997474683060041 ) ;
#11270 = ORIENTED_EDGE ( 'NONE', *, *, #5724, .T. ) ;
#11271 = EDGE_LOOP ( 'NONE', ( #2766, #13343, #10646, #6290 ) ) ;
#11272 = CARTESIAN_POINT ( 'NONE',  ( -0.3969782420128915579, 38.01989097161666109, 9.493666329891928157 ) ) ;
#11273 = EDGE_CURVE ( 'NONE', #11305, #3047, #10379, .T. ) ;
#11274 = DIRECTION ( 'NONE',  ( 0.000000000000000000, 0.000000000000000000, -1.000000000000000000 ) ) ;
#11275 = DIRECTION ( 'NONE',  ( 0.000000000000000000, 0.000000000000000000, -1.000000000000000000 ) ) ;
#11276 = CARTESIAN_POINT ( 'NONE',  ( 25.99999999999996092, 0.000000000000000000, 40.00000000000000711 ) ) ;
#11277 = DIRECTION ( 'NONE',  ( 0.000000000000000000, 0.000000000000000000, -1.000000000000000000 ) ) ;
#11278 = CARTESIAN_POINT ( 'NONE',  ( -40.00000000000000711, 10.00000000000000000, -18.00000000000000355 ) ) ;
#11279 = ADVANCED_FACE ( 'NONE', ( #10122 ), #7692, .T. ) ;
#11280 = AXIS2_PLACEMENT_3D ( 'NONE', #140, #3910, #11641 ) ;
#11281 = ADVANCED_FACE ( 'NONE', ( #3850 ), #5127, .F. ) ;
#11282 = DIRECTION ( 'NONE',  ( -0.000000000000000000, -1.000000000000000000, -0.000000000000000000 ) ) ;
#11283 = EDGE_CURVE ( 'NONE', #10282, #8714, #8017, .T. ) ;
#11284 = LINE ( 'NONE', #11454, #6293 ) ;
#11285 = ORIENTED_EDGE ( 'NONE', *, *, #1483, .T. ) ;
#11286 = DIRECTION ( 'NONE',  ( 1.000000000000000000, -0.000000000000000000, -0.000000000000000000 ) ) ;
#11287 = DIRECTION ( 'NONE',  ( 0.000000000000000000, -1.000000000000000000, 0.000000000000000000 ) ) ;
#11288 = CIRCLE ( 'NONE', #7436, 4.695405383896011919 ) ;
#11289 = LINE ( 'NONE', #11212, #13724 ) ;
#11291 = EDGE_LOOP ( 'NONE', ( #16158, #13405, #772, #14683 ) ) ;
#11290 = VERTEX_POINT ( 'NONE', #14415 ) ;
#11292 = CARTESIAN_POINT ( 'NONE',  ( 31.81980515339464333, 0.000000000000000000, 31.81980515339463622 ) ) ;
#11293 = ORIENTED_EDGE ( 'NONE', *, *, #6014, .T. ) ;
#11294 = VECTOR ( 'NONE', #16760, 1000.000000000000000 ) ;
#11295 = LINE ( 'NONE', #3320, #330 ) ;
#11296 = DIRECTION ( 'NONE',  ( 1.000000000000000000, -0.000000000000000000, 0.000000000000000000 ) ) ;
#11297 = DIRECTION ( 'NONE',  ( -1.000000000000000000, -0.000000000000000000, -0.000000000000000000 ) ) ;
#11298 = ORIENTED_EDGE ( 'NONE', *, *, #12426, .T. ) ;
#11299 = AXIS2_PLACEMENT_3D ( 'NONE', #2822, #2998, #14771 ) ;
#11300 = AXIS2_PLACEMENT_3D ( 'NONE', #6387, #9163, #10289 ) ;
#11301 = DIRECTION ( 'NONE',  ( 1.000000000000000000, 0.000000000000000000, 0.000000000000000000 ) ) ;
#11302 = EDGE_CURVE ( 'NONE', #5839, #3545, #6631, .T. ) ;
#11303 = EDGE_CURVE ( 'NONE', #1082, #7927, #10896, .T. ) ;
#11304 = CARTESIAN_POINT ( 'NONE',  ( 0.000000000000000000, 10.00000000000000000, -12.00000000000000178 ) ) ;
#11305 = VERTEX_POINT ( 'NONE', #8140 ) ;
#11306 = FACE_OUTER_BOUND ( 'NONE', #15790, .T. ) ;
#11307 = EDGE_CURVE ( 'NONE', #8714, #10282, #4461, .T. ) ;
#11308 = DIRECTION ( 'NONE',  ( -1.000000000000000000, -0.000000000000000000, -0.000000000000000000 ) ) ;
#11309 = DIRECTION ( 'NONE',  ( 0.000000000000000000, 0.000000000000000000, -1.000000000000000000 ) ) ;
#11310 = VECTOR ( 'NONE', #11848, 1000.000000000000000 ) ;
#11311 = DIRECTION ( 'NONE',  ( 0.000000000000000000, 0.000000000000000000, -1.000000000000000000 ) ) ;
#11312 = CARTESIAN_POINT ( 'NONE',  ( -31.00000000000005329, 10.00000000000000000, 26.00000000000000000 ) ) ;
#11313 = ORIENTED_EDGE ( 'NONE', *, *, #11927, .F. ) ;
#11314 = DIRECTION ( 'NONE',  ( 0.000000000000000000, 0.000000000000000000, -1.000000000000000000 ) ) ;
#11315 = CIRCLE ( 'NONE', #6354, 9.000000000000007105 ) ;
#11316 = CARTESIAN_POINT ( 'NONE',  ( 35.99999999999999289, 8.000000000000000000, 18.99999999999999289 ) ) ;
#11317 = ORIENTED_EDGE ( 'NONE', *, *, #4952, .T. ) ;
#11318 = LINE ( 'NONE', #12696, #3648 ) ;
#11319 = AXIS2_PLACEMENT_3D ( 'NONE', #14502, #2723, #7957 ) ;
#11320 = VERTEX_POINT ( 'NONE', #13391 ) ;
#11321 = CARTESIAN_POINT ( 'NONE',  ( -8.522270667398414726E-13, 287.0593181834893244, 28.70593181834858498 ) ) ;
#11322 = CARTESIAN_POINT ( 'NONE',  ( 7.000000000000000000, 17.68750000000000000, 0.000000000000000000 ) ) ;
#11323 = ORIENTED_EDGE ( 'NONE', *, *, #3540, .T. ) ;
#11324 = DIRECTION ( 'NONE',  ( -0.000000000000000000, -1.000000000000000000, -0.000000000000000000 ) ) ;
#11325 = VECTOR ( 'NONE', #15409, 1000.000000000000000 ) ;
#11326 = CIRCLE ( 'NONE', #9703, 5.000000000000000888 ) ;
#11327 = CARTESIAN_POINT ( 'NONE',  ( -3.000000000000000000, 41.00000000000000711, 6.000000000000000000 ) ) ;
#11328 = LINE ( 'NONE', #4709, #1265 ) ;
#11329 = VERTEX_POINT ( 'NONE', #1696 ) ;
#11330 = DIRECTION ( 'NONE',  ( 0.000000000000000000, 0.000000000000000000, 1.000000000000000000 ) ) ;
#11331 = CYLINDRICAL_SURFACE ( 'NONE', #5693, 18.50000000000000000 ) ;
#11332 = CARTESIAN_POINT ( 'NONE',  ( 0.7365999999999665038, 289.4632308570086252, 37.52989836422111125 ) ) ;
#11333 = ORIENTED_EDGE ( 'NONE', *, *, #9228, .F. ) ;
#11334 = ORIENTED_EDGE ( 'NONE', *, *, #15234, .T. ) ;
#11335 = CIRCLE ( 'NONE', #3656, 25.25038683781155413 ) ;
#11336 = CARTESIAN_POINT ( 'NONE',  ( -26.00000000000002132, 0.000000000000000000, -31.00000000000003553 ) ) ;
#11337 = APPLICATION_PROTOCOL_DEFINITION ( 'draft international standard', 'automotive_design', 1998, #4459 ) ;
#11338 = CIRCLE ( 'NONE', #15998, 5.000000000000000888 ) ;
#11339 = AXIS2_PLACEMENT_3D ( 'NONE', #11120, #16357, #9836 ) ;
#11340 = ADVANCED_FACE ( 'NONE', ( #9179 ), #5384, .T. ) ;
#11341 = DIRECTION ( 'NONE',  ( 1.000000000000000000, -0.000000000000000000, 0.000000000000000000 ) ) ;
#11342 = EDGE_LOOP ( 'NONE', ( #15983, #3684, #557, #8526 ) ) ;
#11343 = CARTESIAN_POINT ( 'NONE',  ( -39.99999999999997868, 3.000000000000000000, 26.00000000000000355 ) ) ;
#11344 = CARTESIAN_POINT ( 'NONE',  ( 21.00000000000000000, 19.00000000000000000, 31.00000000000006395 ) ) ;
#11345 = VECTOR ( 'NONE', #16668, 1000.000000000000000 ) ;
#11346 = ORIENTED_EDGE ( 'NONE', *, *, #13227, .F. ) ;
#11347 = CARTESIAN_POINT ( 'NONE',  ( 0.000000000000000000, 339.1725919290087745, -10.68226574335978718 ) ) ;
#11348 = DIRECTION ( 'NONE',  ( -0.000000000000000000, -1.000000000000000000, 0.000000000000000000 ) ) ;
#11349 = ORIENTED_EDGE ( 'NONE', *, *, #14128, .F. ) ;
#11350 = PRESENTATION_LAYER_ASSIGNMENT (  '', '', ( #11632 ) ) ;
#11351 = FACE_OUTER_BOUND ( 'NONE', #2936, .T. ) ;
#11352 = VERTEX_POINT ( 'NONE', #2811 ) ;
#11353 = VERTEX_POINT ( 'NONE', #13127 ) ;
#11354 = PRODUCT_RELATED_PRODUCT_CATEGORY ( 'part', '', ( #3694 ) ) ;
#11355 = AXIS2_PLACEMENT_3D ( 'NONE', #8128, #10619, #13378 ) ;
#11356 = ORIENTED_EDGE ( 'NONE', *, *, #13198, .F. ) ;
#11357 = CIRCLE ( 'NONE', #1482, 4.000164074322309027 ) ;
#11358 = PRODUCT_DEFINITION_SHAPE ( 'NONE', 'NONE',  #4018 ) ;
#11359 = ORIENTED_EDGE ( 'NONE', *, *, #2124, .F. ) ;
#11360 = EDGE_CURVE ( 'NONE', #3377, #6787, #12419, .T. ) ;
#11361 = EDGE_LOOP ( 'NONE', ( #1741, #10744, #1904, #15936 ) ) ;
#11363 = FACE_OUTER_BOUND ( 'NONE', #8371, .T. ) ;
#11362 = AXIS2_PLACEMENT_3D ( 'NONE', #10492, #7563, #6523 ) ;
#11364 = VECTOR ( 'NONE', #5579, 1000.000000000000000 ) ;
#11365 = LINE ( 'NONE', #2091, #5793 ) ;
#11366 = LINE ( 'NONE', #4914, #12722 ) ;
#11367 = LINE ( 'NONE', #11530, #8457 ) ;
#11368 = CIRCLE ( 'NONE', #3978, 4.999999999999997335 ) ;
#11369 = PLANE ( 'NONE',  #11056 ) ;
#11370 = DIRECTION ( 'NONE',  ( -1.000000000000000000, 0.000000000000000000, 3.854941057726249930E-16 ) ) ;
#11371 = LINE ( 'NONE', #4842, #15337 ) ;
#11372 = DIRECTION ( 'NONE',  ( 0.000000000000000000, 0.000000000000000000, -1.000000000000000000 ) ) ;
#11373 = VERTEX_POINT ( 'NONE', #5648 ) ;
#11374 = LINE ( 'NONE', #3896, #15830 ) ;
#11375 = DIRECTION ( 'NONE',  ( 0.000000000000000000, -0.000000000000000000, -1.000000000000000000 ) ) ;
#11376 = EDGE_CURVE ( 'NONE', #11430, #6541, #14061, .T. ) ;
#11377 = EDGE_CURVE ( 'NONE', #13903, #7626, #14612, .T. ) ;
#11378 = LINE ( 'NONE', #906, #1367 ) ;
#11380 = ORIENTED_EDGE ( 'NONE', *, *, #5198, .F. ) ;
#11379 = VERTEX_POINT ( 'NONE', #1532 ) ;
#11381 = DIRECTION ( 'NONE',  ( 0.000000000000000000, 0.000000000000000000, 1.000000000000000000 ) ) ;
#11382 = CIRCLE ( 'NONE', #14948, 187.4999999999998863 ) ;
#11383 = ORIENTED_EDGE ( 'NONE', *, *, #11170, .F. ) ;
#11384 = EDGE_CURVE ( 'NONE', #3161, #13435, #1991, .T. ) ;
#11385 = EDGE_CURVE ( 'NONE', #3926, #2958, #15947, .T. ) ;
#11386 = DIRECTION ( 'NONE',  ( 0.000000000000000000, 0.000000000000000000, 1.000000000000000000 ) ) ;
#11387 = EDGE_CURVE ( 'NONE', #2250, #6264, #8851, .T. ) ;
#11388 = CARTESIAN_POINT ( 'NONE',  ( 1.223489862255693833E-15, 0.000000000000000000, -75.00000000000000000 ) ) ;
#11389 = DIRECTION ( 'NONE',  ( -1.000000000000000000, 0.000000000000000000, 0.000000000000000000 ) ) ;
#11390 = EDGE_LOOP ( 'NONE', ( #1271, #9335, #15315, #16281 ) ) ;
#11391 = UNCERTAINTY_MEASURE_WITH_UNIT (LENGTH_MEASURE( 1.000000000000000082E-05 ), #6940, 'distance_accuracy_value', 'NONE');
#11392 = DIRECTION ( 'NONE',  ( 1.000000000000000000, -0.000000000000000000, 0.000000000000000000 ) ) ;
#11393 = CARTESIAN_POINT ( 'NONE',  ( -18.00000000000001421, 6.000000000000000000, 36.00000000000000711 ) ) ;
#11394 = ORIENTED_EDGE ( 'NONE', *, *, #10660, .F. ) ;
#11395 = DIRECTION ( 'NONE',  ( 0.000000000000000000, 0.000000000000000000, -1.000000000000000000 ) ) ;
#11396 = AXIS2_PLACEMENT_3D ( 'NONE', #16119, #15079, #13713 ) ;
#11397 = DIRECTION ( 'NONE',  ( -6.123031769111888756E-17, 1.000000000000000000, 3.749151804555344967E-33 ) ) ;
#11398 = LINE ( 'NONE', #16463, #5824 ) ;
#11399 = EDGE_CURVE ( 'NONE', #14192, #14326, #1353, .T. ) ;
#11400 = CARTESIAN_POINT ( 'NONE',  ( -26.00000000000002132, 10.00000000000000000, 40.00000000000000711 ) ) ;
#11401 = LINE ( 'NONE', #846, #6502 ) ;
#11402 = VERTEX_POINT ( 'NONE', #10804 ) ;
#11403 = LINE ( 'NONE', #16640, #9196 ) ;
#11404 = EDGE_CURVE ( 'NONE', #15749, #5980, #1443, .T. ) ;
#11405 = EDGE_CURVE ( 'NONE', #15841, #11860, #12091, .T. ) ;
#11406 = CONICAL_SURFACE ( 'NONE', #12251, 14.43750000000000000, 0.7483780475235185525 ) ;
#11407 = EDGE_CURVE ( 'NONE', #717, #9546, #362, .T. ) ;
#11408 = CARTESIAN_POINT ( 'NONE',  ( 0.000000000000000000, 425.7506394335853201, 0.000000000000000000 ) ) ;
#11409 = VECTOR ( 'NONE', #9280, 1000.000000000000000 ) ;
#11410 = EDGE_CURVE ( 'NONE', #3442, #16701, #3642, .T. ) ;
#11411 = CARTESIAN_POINT ( 'NONE',  ( -55.99999999999989342, 493.2350855268092573, -585.2659423243250103 ) ) ;
#11412 = ORIENTED_EDGE ( 'NONE', *, *, #11405, .T. ) ;
#11413 = CARTESIAN_POINT ( 'NONE',  ( 394.0000000000001137, 240.7889724647196488, -17.15546574335979813 ) ) ;
#11414 = FACE_OUTER_BOUND ( 'NONE', #7057, .T. ) ;
#11415 = ORIENTED_EDGE ( 'NONE', *, *, #900, .T. ) ;
#11416 = CYLINDRICAL_SURFACE ( 'NONE', #7777, 13.69540538389601991 ) ;
#11417 = DIRECTION ( 'NONE',  ( -1.000000000000000000, -0.000000000000000000, -1.631319816340925608E-17 ) ) ;
#11418 = DIRECTION ( 'NONE',  ( -1.000000000000000000, 0.000000000000000000, -0.000000000000000000 ) ) ;
#11419 = VERTEX_POINT ( 'NONE', #5293 ) ;
#11420 = CIRCLE ( 'NONE', #5662, 9.000000000000007105 ) ;
#11421 = PRESENTATION_STYLE_ASSIGNMENT (( #15294 ) ) ;
#11422 = CARTESIAN_POINT ( 'NONE',  ( -430.0000000000000568, 620.7506394335853201, 0.000000000000000000 ) ) ;
#11423 = DIRECTION ( 'NONE',  ( -0.000000000000000000, 0.000000000000000000, 1.000000000000000000 ) ) ;
#11424 = ORIENTED_EDGE ( 'NONE', *, *, #14796, .T. ) ;
#11425 = CARTESIAN_POINT ( 'NONE',  ( -3.270000000000000462, -25.84985893846420169, 258.4985893846773592 ) ) ;
#11426 = CONTEXT_DEPENDENT_SHAPE_REPRESENTATION ( #8979, #10842 ) ;
#11427 = ADVANCED_FACE ( 'NONE', ( #10546 ), #15779, .F. ) ;
#11428 = CARTESIAN_POINT ( 'NONE',  ( -25.99999999999999645, 68.00000000000000000, 40.00000000000002132 ) ) ;
#11429 = VECTOR ( 'NONE', #11995, 1000.000000000000000 ) ;
#11430 = VERTEX_POINT ( 'NONE', #13866 ) ;
#11431 = CONICAL_SURFACE ( 'NONE', #9520, 12.64907335584850046, 0.003530080289784348537 ) ;
#11432 = DIRECTION ( 'NONE',  ( 0.000000000000000000, -1.000000000000000000, 0.000000000000000000 ) ) ;
#11433 = DIRECTION ( 'NONE',  ( -1.000000000000000000, -0.000000000000000000, -0.000000000000000000 ) ) ;
#11434 = ORIENTED_EDGE ( 'NONE', *, *, #3285, .T. ) ;
#11435 = DIRECTION ( 'NONE',  ( -1.000000000000000000, -0.000000000000000000, -0.000000000000000000 ) ) ;
#11436 = CARTESIAN_POINT ( 'NONE',  ( 3.500000000000000000, -14.59999999999999964, -1.787984326755135766E-15 ) ) ;
#11437 = VERTEX_POINT ( 'NONE', #4748 ) ;
#11438 = CYLINDRICAL_SURFACE ( 'NONE', #6114, 5.000000000000004441 ) ;
#11439 = ADVANCED_FACE ( 'NONE', ( #817 ), #1060, .F. ) ;
#11440 = ORIENTED_EDGE ( 'NONE', *, *, #3019, .F. ) ;
#11441 = VERTEX_POINT ( 'NONE', #10005 ) ;
#11442 = VECTOR ( 'NONE', #8205, 1000.000000000000000 ) ;
#11443 = ORIENTED_EDGE ( 'NONE', *, *, #13051, .T. ) ;
#11444 = EDGE_CURVE ( 'NONE', #13257, #15081, #13533, .T. ) ;
#11445 = ORIENTED_EDGE ( 'NONE', *, *, #2028, .T. ) ;
#11446 = ORIENTED_EDGE ( 'NONE', *, *, #1021, .F. ) ;
#11447 = CARTESIAN_POINT ( 'NONE',  ( 36.99999999999999289, 6.000000000000000000, 22.99999999999999645 ) ) ;
#11448 = CARTESIAN_POINT ( 'NONE',  ( 0.7365999999999665038, 289.4632308570086252, 37.52989836422111125 ) ) ;
#11449 = VECTOR ( 'NONE', #10466, 1000.000000000000000 ) ;
#11450 = CARTESIAN_POINT ( 'NONE',  ( 31.00000000000000000, 19.00000000000000000, -31.00000000000000355 ) ) ;
#11451 = DIRECTION ( 'NONE',  ( 1.000000000000000000, -0.000000000000000000, 0.000000000000000000 ) ) ;
#11452 = DIRECTION ( 'NONE',  ( -0.000000000000000000, -1.000000000000000000, -0.000000000000000000 ) ) ;
#11453 = DIRECTION ( 'NONE',  ( -1.000000000000000000, -0.000000000000000000, -0.000000000000000000 ) ) ;
#11454 = CARTESIAN_POINT ( 'NONE',  ( -55.99999999999989342, 473.6663340069157471, -517.8058340126048051 ) ) ;
#11455 = ORIENTED_EDGE ( 'NONE', *, *, #10615, .T. ) ;
#11456 = CARTESIAN_POINT ( 'NONE',  ( -31.81980515339462912, 11.00000000000000000, 31.81980515339465043 ) ) ;
#11457 = CARTESIAN_POINT ( 'NONE',  ( -23.00000000000002132, 6.000000000000000000, 37.00000000000000711 ) ) ;
#11458 = EDGE_LOOP ( 'NONE', ( #5618, #2299, #12133, #12895 ) ) ;
#11459 = CARTESIAN_POINT ( 'NONE',  ( 39.75350601975127063, 301.2117639810886089, -6.736600000000000144 ) ) ;
#11461 = EDGE_LOOP ( 'NONE', ( #6020, #7159, #15255, #14634 ) ) ;
#11460 = ORIENTED_EDGE ( 'NONE', *, *, #7829, .F. ) ;
#11462 = DIRECTION ( 'NONE',  ( 0.000000000000000000, 1.321694076934710402E-16, -1.000000000000000000 ) ) ;
#11463 = VECTOR ( 'NONE', #5625, 1000.000000000000000 ) ;
#11464 = DIRECTION ( 'NONE',  ( 1.000000000000000000, -0.000000000000000000, 0.000000000000000000 ) ) ;
#11465 = DIRECTION ( 'NONE',  ( 0.000000000000000000, 0.000000000000000000, 1.000000000000000000 ) ) ;
#11466 = FACE_OUTER_BOUND ( 'NONE', #5970, .T. ) ;
#11467 = ORIENTED_EDGE ( 'NONE', *, *, #7924, .F. ) ;
#11468 = ADVANCED_FACE ( 'NONE', ( #9602 ), #15241, .T. ) ;
#11469 = DIRECTION ( 'NONE',  ( 0.000000000000000000, 0.000000000000000000, 1.000000000000000000 ) ) ;
#11470 = CARTESIAN_POINT ( 'NONE',  ( 20.99999999999996092, 0.000000000000000000, 32.50000000000000711 ) ) ;
#11471 = ORIENTED_EDGE ( 'NONE', *, *, #14022, .F. ) ;
#11472 = FACE_OUTER_BOUND ( 'NONE', #11196, .T. ) ;
#11473 = AXIS2_PLACEMENT_3D ( 'NONE', #10462, #6906, #15931 ) ;
#11474 = APPLICATION_CONTEXT ( 'automotive_design' ) ;
#11475 = FACE_BOUND ( 'NONE', #3997, .T. ) ;
#11476 = LINE ( 'NONE', #6304, #14318 ) ;
#11477 = EDGE_CURVE ( 'NONE', #8449, #8929, #2256, .T. ) ;
#11478 = EDGE_CURVE ( 'NONE', #1496, #3722, #10087, .T. ) ;
#11479 = CARTESIAN_POINT ( 'NONE',  ( 75.00000000000000000, 355.3192028797624857, -37.21049682360899169 ) ) ;
#11480 = CARTESIAN_POINT ( 'NONE',  ( 31.00000000000003908, 19.00000000000000000, -26.00000000000000355 ) ) ;
#11481 = ORIENTED_EDGE ( 'NONE', *, *, #4458, .F. ) ;
#11482 = CARTESIAN_POINT ( 'NONE',  ( 0.000000000000000000, 339.3157724647196005, -10.68226574335978718 ) ) ;
#11483 = CYLINDRICAL_SURFACE ( 'NONE', #10739, 13.69540538389601991 ) ;
#11484 = DIRECTION ( 'NONE',  ( -0.000000000000000000, -0.000000000000000000, 1.000000000000000000 ) ) ;
#11485 = VERTEX_POINT ( 'NONE', #12493 ) ;
#11486 = ADVANCED_FACE ( 'NONE', ( #3475 ), #11369, .F. ) ;
#11487 = DIRECTION ( 'NONE',  ( 0.000000000000000000, 1.000000000000000000, 0.000000000000000000 ) ) ;
#11488 = AXIS2_PLACEMENT_3D ( 'NONE', #1679, #13112, #5450 ) ;
#11489 = DIRECTION ( 'NONE',  ( 0.000000000000000000, -0.000000000000000000, 1.000000000000000000 ) ) ;
#11490 = EDGE_LOOP ( 'NONE', ( #7907, #2983 ) ) ;
#11491 = CARTESIAN_POINT ( 'NONE',  ( 0.7366000000000204606, 214.4632308570089947, 287.5298983642209123 ) ) ;
#11492 = EDGE_CURVE ( 'NONE', #14833, #10736, #15402, .T. ) ;
#11493 = DIRECTION ( 'NONE',  ( -1.000000000000000000, 0.000000000000000000, 0.000000000000000000 ) ) ;
#11494 = CARTESIAN_POINT ( 'NONE',  ( 55.99999999999989342, 559.9933750504617365, -546.7230258972048205 ) ) ;
#11495 = FACE_OUTER_BOUND ( 'NONE', #7221, .T. ) ;
#11496 = EDGE_CURVE ( 'NONE', #2454, #1299, #2273, .T. ) ;
#11497 = EDGE_CURVE ( 'NONE', #4223, #4316, #2094, .T. ) ;
#11498 = EDGE_CURVE ( 'NONE', #11860, #4422, #981, .T. ) ;
#11499 =( NAMED_UNIT ( * ) SI_UNIT ( $, .STERADIAN. ) SOLID_ANGLE_UNIT ( ) );
#11500 = DIRECTION ( 'NONE',  ( 1.000000000000000000, -0.000000000000000000, -0.000000000000000000 ) ) ;
#11501 = DIRECTION ( 'NONE',  ( -0.000000000000000000, 1.000000000000000000, -0.000000000000000000 ) ) ;
#11502 = VERTEX_POINT ( 'NONE', #13562 ) ;
#11503 = FACE_OUTER_BOUND ( 'NONE', #8012, .T. ) ;
#11504 = AXIS2_PLACEMENT_3D ( 'NONE', #12361, #601, #13737 ) ;
#11505 =( LENGTH_UNIT ( ) NAMED_UNIT ( * ) SI_UNIT ( .MILLI., .METRE. ) );
#11506 = ORIENTED_EDGE ( 'NONE', *, *, #9286, .T. ) ;
#11507 = LINE ( 'NONE', #6333, #9949 ) ;
#11508 = DIRECTION ( 'NONE',  ( 6.123031769111888756E-17, 0.000000000000000000, 1.000000000000000000 ) ) ;
#11509 = LINE ( 'NONE', #4976, #8232 ) ;
#11510 = ORIENTED_EDGE ( 'NONE', *, *, #6493, .T. ) ;
#11511 = CARTESIAN_POINT ( 'NONE',  ( 40.00000000000000711, 11.00000000000000000, -26.00000000000000355 ) ) ;
#11512 = EDGE_CURVE ( 'NONE', #6709, #4587, #2176, .T. ) ;
#11513 = CARTESIAN_POINT ( 'NONE',  ( 25.99999999999997868, 8.000000000000000000, -39.99999999999999289 ) ) ;
#11514 = ORIENTED_EDGE ( 'NONE', *, *, #8682, .F. ) ;
#11515 = VECTOR ( 'NONE', #16286, 1000.000000000000000 ) ;
#11516 = AXIS2_PLACEMENT_3D ( 'NONE', #10439, #6473, #9161 ) ;
#11517 = EDGE_CURVE ( 'NONE', #11889, #4981, #16605, .T. ) ;
#11518 = DIRECTION ( 'NONE',  ( 0.000000000000000000, 0.000000000000000000, -1.000000000000000000 ) ) ;
#11519 = ORIENTED_EDGE ( 'NONE', *, *, #8088, .T. ) ;
#11520 = ORIENTED_EDGE ( 'NONE', *, *, #8483, .F. ) ;
#11521 = CARTESIAN_POINT ( 'NONE',  ( 46.99999999999988631, 473.6663340069158039, -575.6402177818052905 ) ) ;
#11522 = ORIENTED_EDGE ( 'NONE', *, *, #5099, .F. ) ;
#11523 = DIRECTION ( 'NONE',  ( 1.000000000000000000, 0.000000000000000000, 0.000000000000000000 ) ) ;
#11524 = ORIENTED_EDGE ( 'NONE', *, *, #6418, .F. ) ;
#11525 = VECTOR ( 'NONE', #7498, 1000.000000000000000 ) ;
#11526 = VERTEX_POINT ( 'NONE', #3644 ) ;
#11527 = CIRCLE ( 'NONE', #265, 18.50000000000000000 ) ;
#11528 = DIRECTION ( 'NONE',  ( -1.000000000000000000, 6.123233995735932031E-18, -1.353873099427752636E-32 ) ) ;
#11529 = DIRECTION ( 'NONE',  ( 1.000000000000000000, -0.000000000000000000, -0.000000000000000000 ) ) ;
#11530 = CARTESIAN_POINT ( 'NONE',  ( -2.220446049250313081E-13, 135.5000000000000000, 3.000000000000000000 ) ) ;
#11531 = DIRECTION ( 'NONE',  ( -0.000000000000000000, 1.000000000000000000, -0.000000000000000000 ) ) ;
#11532 = LINE ( 'NONE', #12658, #1074 ) ;
#11533 = CARTESIAN_POINT ( 'NONE',  ( 0.000000000000000000, 339.1725919290084335, -111.4188657433597456 ) ) ;
#11534 = ORIENTED_EDGE ( 'NONE', *, *, #14654, .T. ) ;
#11535 = CARTESIAN_POINT ( 'NONE',  ( 0.000000000000000000, 226.8713558223388134, -333.7582248962859808 ) ) ;
#11536 = DIRECTION ( 'NONE',  ( -1.000000000000000000, -0.000000000000000000, -0.000000000000000000 ) ) ;
#11537 = ORIENTED_EDGE ( 'NONE', *, *, #16704, .T. ) ;
#11538 = CIRCLE ( 'NONE', #2486, 22.75209553982837463 ) ;
#11539 = DIRECTION ( 'NONE',  ( -0.000000000000000000, -1.000000000000000000, 0.000000000000000000 ) ) ;
#11541 = ORIENTED_EDGE ( 'NONE', *, *, #2816, .T. ) ;
#11540 = VERTEX_POINT ( 'NONE', #12748 ) ;
#11542 = DIRECTION ( 'NONE',  ( 0.000000000000000000, 0.000000000000000000, 1.000000000000000000 ) ) ;
#11543 = VERTEX_POINT ( 'NONE', #5960 ) ;
#11544 = CARTESIAN_POINT ( 'NONE',  ( -25.99999999999999645, 68.00000000000000000, 40.00000000000002132 ) ) ;
#11545 = DIRECTION ( 'NONE',  ( -0.000000000000000000, -1.000000000000000000, -0.000000000000000000 ) ) ;
#11546 = FACE_OUTER_BOUND ( 'NONE', #9958, .T. ) ;
#11547 = AXIS2_PLACEMENT_3D ( 'NONE', #10778, #13281, #1509 ) ;
#11548 = ORIENTED_EDGE ( 'NONE', *, *, #11865, .F. ) ;
#11549 = DIRECTION ( 'NONE',  ( 1.000000000000000000, 0.000000000000000000, 0.000000000000000000 ) ) ;
#11550 = ORIENTED_EDGE ( 'NONE', *, *, #4156, .T. ) ;
#11551 = CYLINDRICAL_SURFACE ( 'NONE', #11516, 187.4999999999998863 ) ;
#11552 = CIRCLE ( 'NONE', #11853, 3.300000000000004263 ) ;
#11553 = AXIS2_PLACEMENT_3D ( 'NONE', #4099, #12003, #8212 ) ;
#11554 = DIRECTION ( 'NONE',  ( -1.000000000000000000, 0.000000000000000000, 0.000000000000000000 ) ) ;
#11555 = DIRECTION ( 'NONE',  ( -1.000000000000000000, 0.000000000000000000, 0.000000000000000000 ) ) ;
#11556 = CARTESIAN_POINT ( 'NONE',  ( -22.00000000000001776, 8.000000000000000000, 33.00000000000000711 ) ) ;
#11557 = DIRECTION ( 'NONE',  ( 0.000000000000000000, 1.000000000000000000, 0.000000000000000000 ) ) ;
#11558 = ORIENTED_EDGE ( 'NONE', *, *, #5032, .F. ) ;
#11559 = CIRCLE ( 'NONE', #6331, 59.99999999999994316 ) ;
#11560 = CARTESIAN_POINT ( 'NONE',  ( 0.000000000000000000, 38.00000000000000711, 0.9999999999999943379 ) ) ;
#11561 = EDGE_CURVE ( 'NONE', #4414, #5863, #895, .T. ) ;
#11562 = CIRCLE ( 'NONE', #7715, 13.69540538389601991 ) ;
#11563 = DIRECTION ( 'NONE',  ( 0.000000000000000000, 0.000000000000000000, 1.000000000000000000 ) ) ;
#11564 = AXIS2_PLACEMENT_3D ( 'NONE', #1341, #8997, #3762 ) ;
#11565 = VECTOR ( 'NONE', #8560, 1000.000000000000000 ) ;
#11566 = FACE_OUTER_BOUND ( 'NONE', #13529, .T. ) ;
#11567 = ADVANCED_FACE ( 'NONE', ( #7239 ), #8884, .T. ) ;
#11568 = VERTEX_POINT ( 'NONE', #6118 ) ;
#11569 = DIRECTION ( 'NONE',  ( 1.000000000000000000, 0.000000000000000000, 0.000000000000000000 ) ) ;
#11570 = AXIS2_PLACEMENT_3D ( 'NONE', #15382, #13065, #6178 ) ;
#11571 = CARTESIAN_POINT ( 'NONE',  ( -46.99999999999988631, 473.6663340069157471, -531.5012393965008641 ) ) ;
#11572 = VERTEX_POINT ( 'NONE', #14033 ) ;
#11573 = CARTESIAN_POINT ( 'NONE',  ( -23.00000000000002132, 0.000000000000000000, 37.00000000000000711 ) ) ;
#11574 = DIRECTION ( 'NONE',  ( -1.000000000000000000, 0.000000000000000000, 0.000000000000000000 ) ) ;
#11575 = DIRECTION ( 'NONE',  ( 0.000000000000000000, -1.000000000000000000, -0.000000000000000000 ) ) ;
#11576 = ORIENTED_EDGE ( 'NONE', *, *, #1266, .T. ) ;
#11577 = VECTOR ( 'NONE', #6741, 1000.000000000000114 ) ;
#11578 = CARTESIAN_POINT ( 'NONE',  ( 0.7365999999999761627, 261.2094592450197297, 287.2045212030218408 ) ) ;
#11579 = VECTOR ( 'NONE', #5105, 1000.000000000000000 ) ;
#11580 = DIRECTION ( 'NONE',  ( 0.000000000000000000, 0.000000000000000000, 1.000000000000000000 ) ) ;
#11581 = ORIENTED_EDGE ( 'NONE', *, *, #6779, .F. ) ;
#11582 = DIRECTION ( 'NONE',  ( -1.000000000000000000, 0.000000000000000000, 0.000000000000000000 ) ) ;
#11583 = ADVANCED_FACE ( 'NONE', ( #7572 ), #9915, .T. ) ;
#11584 = ADVANCED_FACE ( 'NONE', ( #5244 ), #14623, .T. ) ;
#11585 = CIRCLE ( 'NONE', #12697, 5.000000000000004441 ) ;
#11586 = EDGE_CURVE ( 'NONE', #750, #6348, #4068, .T. ) ;
#11587 = VECTOR ( 'NONE', #11372, 1000.000000000000000 ) ;
#11588 = EDGE_CURVE ( 'NONE', #16590, #13450, #5013, .T. ) ;
#11589 = VERTEX_POINT ( 'NONE', #8967 ) ;
#11590 = EDGE_CURVE ( 'NONE', #3569, #2956, #5164, .T. ) ;
#11591 = CIRCLE ( 'NONE', #9664, 18.50000000000000000 ) ;
#11592 = CARTESIAN_POINT ( 'NONE',  ( 35.00000000000003553, 0.000000000000000000, -23.50000000000000000 ) ) ;
#11593 = CARTESIAN_POINT ( 'NONE',  ( 394.0000000000001137, 339.1725919290084335, -110.6822657433597925 ) ) ;
#11594 = FACE_OUTER_BOUND ( 'NONE', #16919, .T. ) ;
#11595 = VERTEX_POINT ( 'NONE', #5087 ) ;
#11596 = DIRECTION ( 'NONE',  ( 0.000000000000000000, 1.000000000000000000, 0.000000000000000000 ) ) ;
#11597 = CARTESIAN_POINT ( 'NONE',  ( 6.649999999999999467, 0.000000000000000000, 0.000000000000000000 ) ) ;
#11598 = ORIENTED_EDGE ( 'NONE', *, *, #16355, .T. ) ;
#11599 = VECTOR ( 'NONE', #3890, 1000.000000000000000 ) ;
#11600 = FACE_OUTER_BOUND ( 'NONE', #15864, .T. ) ;
#11601 = EDGE_LOOP ( 'NONE', ( #16297, #16593 ) ) ;
#11602 = ORIENTED_EDGE ( 'NONE', *, *, #12447, .F. ) ;
#11603 = VECTOR ( 'NONE', #15906, 1000.000000000000000 ) ;
#11604 = CARTESIAN_POINT ( 'NONE',  ( 39.99999999999999289, 0.000000000000000000, -26.00000000000000000 ) ) ;
#11605 = VECTOR ( 'NONE', #9584, 1000.000000000000000 ) ;
#11606 = VECTOR ( 'NONE', #6314, 1000.000000000000227 ) ;
#11607 = VERTEX_POINT ( 'NONE', #2685 ) ;
#11608 = ORIENTED_EDGE ( 'NONE', *, *, #7610, .T. ) ;
#11609 = EDGE_CURVE ( 'NONE', #2613, #11485, #2767, .T. ) ;
#11610 = AXIS2_PLACEMENT_3D ( 'NONE', #10652, #10916, #8246 ) ;
#11611 = EDGE_CURVE ( 'NONE', #11779, #9431, #3124, .T. ) ;
#11612 = EDGE_LOOP ( 'NONE', ( #13683, #9645 ) ) ;
#11613 = EDGE_CURVE ( 'NONE', #14988, #14016, #6616, .T. ) ;
#11614 = CARTESIAN_POINT ( 'NONE',  ( -18.00000000000001421, 10.00000000000000000, 40.00000000000000711 ) ) ;
#11615 = FACE_OUTER_BOUND ( 'NONE', #586, .T. ) ;
#11616 = AXIS2_PLACEMENT_3D ( 'NONE', #12310, #8782, #8616 ) ;
#11617 = AXIS2_PLACEMENT_3D ( 'NONE', #5782, #4252, #16006 ) ;
#11618 = VERTEX_POINT ( 'NONE', #3730 ) ;
#11619 = DIRECTION ( 'NONE',  ( 1.000000000000000000, -0.000000000000000000, 0.000000000000000000 ) ) ;
#11620 = CIRCLE ( 'NONE', #12448, 187.4999999999998863 ) ;
#11621 = DIRECTION ( 'NONE',  ( 0.000000000000000000, -1.000000000000000000, 0.000000000000000000 ) ) ;
#11622 = ADVANCED_BREP_SHAPE_REPRESENTATION ( '', ( #3244, #1488 ), #16822 ) ;
#11623 = VECTOR ( 'NONE', #1302, 1000.000000000000000 ) ;
#11624 = DIRECTION ( 'NONE',  ( 1.000000000000000000, 0.000000000000000000, 0.000000000000000000 ) ) ;
#11625 = ORIENTED_EDGE ( 'NONE', *, *, #3971, .T. ) ;
#11626 = LINE ( 'NONE', #14287, #13910 ) ;
#11627 = LINE ( 'NONE', #2430, #15170 ) ;
#11628 = AXIS2_PLACEMENT_3D ( 'NONE', #9013, #6578, #16650 ) ;
#11629 = ORIENTED_EDGE ( 'NONE', *, *, #7274, .T. ) ;
#11630 = CARTESIAN_POINT ( 'NONE',  ( 22.99999999999997513, 10.00000000000000000, 31.00000000000005684 ) ) ;
#11631 = VERTEX_POINT ( 'NONE', #2506 ) ;
#11632 = STYLED_ITEM ( 'NONE', ( #359 ), #3067 ) ;
#11633 = LINE ( 'NONE', #14216, #6443 ) ;
#11634 = AXIS2_PLACEMENT_3D ( 'NONE', #5682, #5500, #10745 ) ;
#11635 = AXIS2_PLACEMENT_3D ( 'NONE', #8095, #15734, #1393 ) ;
#11636 = EDGE_LOOP ( 'NONE', ( #11317, #471, #7295, #4391, #14648, #11412, #15859, #6604, #5324, #7202, #211, #5505, #7862, #1136, #7200, #14113 ) ) ;
#11637 = ORIENTED_EDGE ( 'NONE', *, *, #2005, .F. ) ;
#11638 = CARTESIAN_POINT ( 'NONE',  ( 10.00000000000000000, 364.9870314427752191, -206.3519347178565795 ) ) ;
#11639 = VECTOR ( 'NONE', #14426, 1000.000000000000000 ) ;
#11640 = VECTOR ( 'NONE', #8745, 1000.000000000000000 ) ;
#11641 = DIRECTION ( 'NONE',  ( 0.000000000000000000, 0.000000000000000000, -1.000000000000000000 ) ) ;
#11642 = DIRECTION ( 'NONE',  ( 1.000000000000000000, 0.000000000000000000, 0.000000000000000000 ) ) ;
#11643 = VERTEX_POINT ( 'NONE', #2423 ) ;
#11644 = CARTESIAN_POINT ( 'NONE',  ( -26.00000000000002842, 3.000000000000000000, -39.99999999999999289 ) ) ;
#11645 = DIRECTION ( 'NONE',  ( 0.000000000000000000, 0.000000000000000000, -1.000000000000000000 ) ) ;
#11646 = PRODUCT_DEFINITION_FORMATION_WITH_SPECIFIED_SOURCE ( 'ANY', '', #4910, .NOT_KNOWN. ) ;
#11647 = FACE_OUTER_BOUND ( 'NONE', #3266, .T. ) ;
#11648 = CARTESIAN_POINT ( 'NONE',  ( 0.000000000000000000, 240.7889724647196488, -110.6822657433598067 ) ) ;
#11649 = CARTESIAN_POINT ( 'NONE',  ( 75.00000000000000000, 380.0000000000000000, 0.000000000000000000 ) ) ;
#11650 = VECTOR ( 'NONE', #9446, 1000.000000000000000 ) ;
#11651 = DIRECTION ( 'NONE',  ( 0.000000000000000000, 0.000000000000000000, 1.000000000000000000 ) ) ;
#11652 = LINE ( 'NONE', #9074, #12826 ) ;
#11654 = ORIENTED_EDGE ( 'NONE', *, *, #566, .F. ) ;
#11653 = ORIENTED_EDGE ( 'NONE', *, *, #12023, .F. ) ;
#11655 = LINE ( 'NONE', #8827, #12776 ) ;
#11656 = EDGE_CURVE ( 'NONE', #2908, #785, #11335, .T. ) ;
#11657 = LINE ( 'NONE', #15439, #15946 ) ;
#11658 = LINE ( 'NONE', #8923, #15701 ) ;
#11659 = ORIENTED_EDGE ( 'NONE', *, *, #8989, .F. ) ;
#11660 = AXIS2_PLACEMENT_3D ( 'NONE', #12085, #324, #14756 ) ;
#11661 = CARTESIAN_POINT ( 'NONE',  ( -45.00000000000000000, 493.2350855268092573, -571.5705369404290650 ) ) ;
#11662 = PRODUCT_RELATED_PRODUCT_CATEGORY ( 'part', '', ( #1080 ) ) ;
#11663 = FACE_OUTER_BOUND ( 'NONE', #10681, .T. ) ;
#11664 = ORIENTED_EDGE ( 'NONE', *, *, #4665, .T. ) ;
#11665 = DIRECTION ( 'NONE',  ( 0.000000000000000000, 0.09950371902099953980, 0.9950371902099890420 ) ) ;
#11666 = CYLINDRICAL_SURFACE ( 'NONE', #1056, 3.999999999999996447 ) ;
#11667 = PLANE ( 'NONE',  #6180 ) ;
#11668 = CARTESIAN_POINT ( 'NONE',  ( 10.00000000000000000, 411.2412070270587492, -605.3473189749742005 ) ) ;
#11669 = CARTESIAN_POINT ( 'NONE',  ( 25.99999999999996092, 0.000000000000000000, -31.00000000000003197 ) ) ;
#11670 = DIRECTION ( 'NONE',  ( -1.000000000000000000, -0.000000000000000000, -0.000000000000000000 ) ) ;
#11671 = CARTESIAN_POINT ( 'NONE',  ( 0.000000000000000000, 339.1725919290084335, -104.9456657433597968 ) ) ;
#11672 = VERTEX_POINT ( 'NONE', #15648 ) ;
#11673 = EDGE_CURVE ( 'NONE', #1004, #12140, #5571, .T. ) ;
#11674 = VECTOR ( 'NONE', #1989, 1000.000000000000000 ) ;
#11675 = CARTESIAN_POINT ( 'NONE',  ( 0.000000000000000000, 0.000000000000000000, 3.000000000000000000 ) ) ;
#11676 = CIRCLE ( 'NONE', #991, 15.14120580695350071 ) ;
#11677 = ITEM_DEFINED_TRANSFORMATION ( 'NONE', 'NONE', #11617,  #1488 ) ;
#11678 =( LENGTH_UNIT ( ) NAMED_UNIT ( * ) SI_UNIT ( .MILLI., .METRE. ) );
#11679 = CARTESIAN_POINT ( 'NONE',  ( 31.00000000000001421, 6.000000000000000000, 22.99999999999999645 ) ) ;
#11680 = VERTEX_POINT ( 'NONE', #3989 ) ;
#11681 = DIRECTION ( 'NONE',  ( -1.000000000000000000, -0.000000000000000000, -0.000000000000000000 ) ) ;
#11682 = DIRECTION ( 'NONE',  ( 6.123031769111888756E-17, 0.000000000000000000, 1.000000000000000000 ) ) ;
#11683 = VECTOR ( 'NONE', #13587, 1000.000000000000000 ) ;
#11684 = EDGE_CURVE ( 'NONE', #2977, #10067, #14540, .T. ) ;
#11685 = CARTESIAN_POINT ( 'NONE',  ( -22.00000000000001776, 10.00000000000000000, 36.00000000000000711 ) ) ;
#11686 = EDGE_LOOP ( 'NONE', ( #10970, #1836, #5681, #15012 ) ) ;
#11687 = CONICAL_SURFACE ( 'NONE', #2918, 12.97499999999999964, 0.5543074962015517304 ) ;
#11688 = FACE_OUTER_BOUND ( 'NONE', #5651, .T. ) ;
#11689 = DIRECTION ( 'NONE',  ( -1.000000000000000000, 0.000000000000000000, 0.000000000000000000 ) ) ;
#11690 = ORIENTED_EDGE ( 'NONE', *, *, #12548, .T. ) ;
#11691 = DIRECTION ( 'NONE',  ( 7.213771534993947851E-17, 0.09950371902098976984, 0.9950371902099900412 ) ) ;
#11692 = ORIENTED_EDGE ( 'NONE', *, *, #7392, .F. ) ;
#11693 = ORIENTED_EDGE ( 'NONE', *, *, #11825, .T. ) ;
#11694 = EDGE_CURVE ( 'NONE', #3043, #8801, #13258, .T. ) ;
#11695 = DIRECTION ( 'NONE',  ( -1.000000000000000000, -0.000000000000000000, -0.000000000000000000 ) ) ;
#11696 = VERTEX_POINT ( 'NONE', #5000 ) ;
#11697 = AXIS2_PLACEMENT_3D ( 'NONE', #4942, #10194, #7599 ) ;
#11698 = CIRCLE ( 'NONE', #6765, 8.000000000000000000 ) ;
#11699 = ORIENTED_EDGE ( 'NONE', *, *, #3237, .F. ) ;
#11700 = ORIENTED_EDGE ( 'NONE', *, *, #1261, .T. ) ;
#11701 = CARTESIAN_POINT ( 'NONE',  ( 0.7366000000000112458, 193.4499468633054846, 37.13122676359123631 ) ) ;
#11702 = FACE_OUTER_BOUND ( 'NONE', #8657, .T. ) ;
#11703 =( REPRESENTATION_RELATIONSHIP ('NONE','NONE', #15277, #1883 ) REPRESENTATION_RELATIONSHIP_WITH_TRANSFORMATION ( #2653 )SHAPE_REPRESENTATION_RELATIONSHIP( ) );
#11704 = EDGE_CURVE ( 'NONE', #4673, #11, #3809, .T. ) ;
#11705 = ORIENTED_EDGE ( 'NONE', *, *, #1549, .F. ) ;
#11706 = CARTESIAN_POINT ( 'NONE',  ( 10.00000000000000000, -156.2292101480469739, -357.0417483806770633 ) ) ;
#11707 = AXIS2_PLACEMENT_3D ( 'NONE', #14999, #15154, #4754 ) ;
#11708 = VECTOR ( 'NONE', #7556, 1000.000000000000000 ) ;
#11709 = DIRECTION ( 'NONE',  ( -1.000000000000000000, 0.000000000000000000, 0.000000000000000000 ) ) ;
#11710 = EDGE_CURVE ( 'NONE', #13693, #16255, #14205, .T. ) ;
#11711 = EDGE_LOOP ( 'NONE', ( #10655, #2845, #11839, #7359 ) ) ;
#11712 = DIRECTION ( 'NONE',  ( 1.000000000000000000, -0.000000000000000000, -0.000000000000000000 ) ) ;
#11713 = DIRECTION ( 'NONE',  ( 1.000000000000000000, 0.000000000000000000, -0.000000000000000000 ) ) ;
#11714 = ORIENTED_EDGE ( 'NONE', *, *, #11302, .T. ) ;
#11715 = EDGE_CURVE ( 'NONE', #11859, #7947, #15721, .T. ) ;
#11716 = ADVANCED_FACE ( 'NONE', ( #15494 ), #14912, .F. ) ;
#11717 = EDGE_CURVE ( 'NONE', #5545, #3569, #12169, .T. ) ;
#11718 = CARTESIAN_POINT ( 'NONE',  ( 22.99999999999998224, 0.000000000000000000, -36.99999999999999289 ) ) ;
#11719 = ORIENTED_EDGE ( 'NONE', *, *, #11477, .T. ) ;
#11720 = DIRECTION ( 'NONE',  ( 1.000000000000000000, 0.000000000000000000, 0.000000000000000000 ) ) ;
#11721 = ORIENTED_EDGE ( 'NONE', *, *, #9068, .F. ) ;
#11722 = AXIS2_PLACEMENT_3D ( 'NONE', #7370, #15369, #7540 ) ;
#11723 = ORIENTED_EDGE ( 'NONE', *, *, #4967, .F. ) ;
#11724 =( LENGTH_UNIT ( ) NAMED_UNIT ( * ) SI_UNIT ( .MILLI., .METRE. ) );
#11725 = DIRECTION ( 'NONE',  ( -1.000000000000000000, -0.000000000000000000, 0.000000000000000000 ) ) ;
#11726 = DIRECTION ( 'NONE',  ( -0.000000000000000000, -0.000000000000000000, 1.000000000000000000 ) ) ;
#11727 = EDGE_LOOP ( 'NONE', ( #5387, #2500, #9659, #4716, #5813, #5441, #15025, #16823, #534, #9467, #14300, #5120, #10402, #9281, #835, #11240 ) ) ;
#11728 = CARTESIAN_POINT ( 'NONE',  ( 54.99999999999999289, 515.4878487013597805, -546.7230258972048205 ) ) ;
#11729 = PLANE ( 'NONE',  #8038 ) ;
#11730 = B_SPLINE_CURVE_WITH_KNOTS ( 'NONE', 3,
 ( #5306, #5214, #2474, #10638, #86, #15622 ),
 .UNSPECIFIED., .F., .F.,
 ( 4, 2, 4 ),
 ( 0.000000000000000000, 0.5000000000000000000, 1.000000000000000000 ),
 .UNSPECIFIED. ) ;
#11731 = CARTESIAN_POINT ( 'NONE',  ( -26.00000000000002842, 3.000000000000000000, 34.00000000000000711 ) ) ;
#11732 = DIRECTION ( 'NONE',  ( 0.000000000000000000, 0.000000000000000000, -1.000000000000000000 ) ) ;
#11733 = FACE_OUTER_BOUND ( 'NONE', #10703, .T. ) ;
#11734 = COLOUR_RGB ( '', 0.72549020, 0.75294118, 0.79215686) ;
#11735 = EDGE_CURVE ( 'NONE', #1501, #10013, #1235, .T. ) ;
#11736 = ADVANCED_FACE ( 'NONE', ( #1834 ), #11874, .F. ) ;
#11737 = DIRECTION ( 'NONE',  ( -1.597771622610217359E-16, 1.000000000000000000, -0.000000000000000000 ) ) ;
#11738 = AXIS2_PLACEMENT_3D ( 'NONE', #4350, #16107, #1596 ) ;
#11739 = CARTESIAN_POINT ( 'NONE',  ( 0.7366000000000112458, 193.4499468633054846, 37.13122676359123631 ) ) ;
#11741 = ORIENTED_EDGE ( 'NONE', *, *, #16844, .F. ) ;
#11740 = ORIENTED_EDGE ( 'NONE', *, *, #8964, .T. ) ;
#11742 = DIRECTION ( 'NONE',  ( -0.000000000000000000, -0.000000000000000000, 1.000000000000000000 ) ) ;
#11743 = CARTESIAN_POINT ( 'NONE',  ( 10.00000000000000000, 425.7506394335853201, -11.00000000000000000 ) ) ;
#11744 = DIRECTION ( 'NONE',  ( -1.000000000000000000, -0.000000000000000000, -0.000000000000000000 ) ) ;
#11745 = ORIENTED_EDGE ( 'NONE', *, *, #16780, .F. ) ;
#11746 = AXIS2_PLACEMENT_3D ( 'NONE', #2136, #7364, #858 ) ;
#11747 = CARTESIAN_POINT ( 'NONE',  ( -5.000000000000000888, 0.000000000000000000, 0.000000000000000000 ) ) ;
#11748 = EDGE_CURVE ( 'NONE', #13878, #11353, #13519, .T. ) ;
#11749 = DIRECTION ( 'NONE',  ( 0.000000000000000000, 0.3420201433256759294, -0.9396926207859057634 ) ) ;
#11750 = ORIENTED_EDGE ( 'NONE', *, *, #13369, .F. ) ;
#11751 = DIRECTION ( 'NONE',  ( 0.000000000000000000, -1.000000000000000000, 0.000000000000000000 ) ) ;
#11752 = CARTESIAN_POINT ( 'NONE',  ( 30.99999999999996092, 3.000000000000000000, -30.99999999999999289 ) ) ;
#11753 = PLANE ( 'NONE',  #5367 ) ;
#11754 = ORIENTED_EDGE ( 'NONE', *, *, #12878, .T. ) ;
#11755 = SURFACE_SIDE_STYLE ('',( #7791 ) ) ;
#11756 = DIRECTION ( 'NONE',  ( 0.000000000000000000, -1.000000000000000000, -7.137148015447440312E-15 ) ) ;
#11757 = CARTESIAN_POINT ( 'NONE',  ( 31.00000000000002842, 68.00000000000000000, 23.00000000000001066 ) ) ;
#11758 = EDGE_LOOP ( 'NONE', ( #1909, #14189, #15557, #16925 ) ) ;
#11759 = DIRECTION ( 'NONE',  ( 1.000000000000000000, 0.000000000000000000, 0.000000000000000000 ) ) ;
#11760 = CIRCLE ( 'NONE', #10111, 6.473200000000002063 ) ;
#11761 = SHAPE_REPRESENTATION ( 'Part9', ( #1488 ), #14386 ) ;
#11762 = DIRECTION ( 'NONE',  ( -0.000000000000000000, -1.000000000000000000, -0.000000000000000000 ) ) ;
#11763 = VERTEX_POINT ( 'NONE', #10934 ) ;
#11764 = DIRECTION ( 'NONE',  ( -0.000000000000000000, -0.000000000000000000, 1.000000000000000000 ) ) ;
#11765 = FACE_OUTER_BOUND ( 'NONE', #14514, .T. ) ;
#11766 = DIRECTION ( 'NONE',  ( 0.000000000000000000, 0.000000000000000000, -1.000000000000000000 ) ) ;
#11767 = ORIENTED_EDGE ( 'NONE', *, *, #12880, .T. ) ;
#11768 = CARTESIAN_POINT ( 'NONE',  ( 10.00000000000000000, 214.9999999999953104, -486.7326477857724853 ) ) ;
#11769 = DIRECTION ( 'NONE',  ( -1.000000000000000000, 0.000000000000000000, 0.000000000000000000 ) ) ;
#11770 = CYLINDRICAL_SURFACE ( 'NONE', #754, 34.00000000000000000 ) ;
#11771 = ORIENTED_EDGE ( 'NONE', *, *, #404, .T. ) ;
#11772 = DIRECTION ( 'NONE',  ( 0.000000000000000000, 0.000000000000000000, 1.000000000000000000 ) ) ;
#11773 = ORIENTED_EDGE ( 'NONE', *, *, #5520, .T. ) ;
#11774 = EDGE_LOOP ( 'NONE', ( #638, #4502, #15910, #1238 ) ) ;
#11775 = DIRECTION ( 'NONE',  ( -0.000000000000000000, -1.000000000000000000, -0.000000000000000000 ) ) ;
#11776 = VERTEX_POINT ( 'NONE', #6971 ) ;
#11777 = DIRECTION ( 'NONE',  ( 0.000000000000000000, 0.000000000000000000, 1.000000000000000000 ) ) ;
#11778 = ADVANCED_FACE ( 'NONE', ( #14974, #8099 ), #8444, .F. ) ;
#11779 = VERTEX_POINT ( 'NONE', #15903 ) ;
#11780 = ORIENTED_EDGE ( 'NONE', *, *, #1848, .T. ) ;
#11781 = DIRECTION ( 'NONE',  ( -7.213771534993946619E-17, -0.09950371902098976984, -0.9950371902099900412 ) ) ;
#11782 = CARTESIAN_POINT ( 'NONE',  ( -25.99999999999999645, 68.00000000000000000, -39.99999999999999289 ) ) ;
#11783 = EDGE_CURVE ( 'NONE', #4127, #1137, #16165, .T. ) ;
#11784 = VECTOR ( 'NONE', #2890, 1000.000000000000000 ) ;
#11785 = ORIENTED_EDGE ( 'NONE', *, *, #8857, .T. ) ;
#11787 = DIRECTION ( 'NONE',  ( 0.000000000000000000, 0.000000000000000000, -1.000000000000000000 ) ) ;
#11786 = AXIS2_PLACEMENT_3D ( 'NONE', #10899, #15950, #10808 ) ;
#11788 = FACE_OUTER_BOUND ( 'NONE', #1825, .T. ) ;
#11789 = DIRECTION ( 'NONE',  ( 0.000000000000000000, 0.000000000000000000, -1.000000000000000000 ) ) ;
#11790 = ORIENTED_EDGE ( 'NONE', *, *, #12530, .T. ) ;
#11791 = CARTESIAN_POINT ( 'NONE',  ( 18.99999999999998224, 8.000000000000000000, -35.99999999999999289 ) ) ;
#11792 = CARTESIAN_POINT ( 'NONE',  ( 10.00000000000000000, 620.7506394335853201, -11.00000000000000000 ) ) ;
#11793 = ADVANCED_BREP_SHAPE_REPRESENTATION ( '', ( #14168, #1488 ), #3145 ) ;
#11794 = ORIENTED_EDGE ( 'NONE', *, *, #13617, .F. ) ;
#11795 = CARTESIAN_POINT ( 'NONE',  ( 55.99999999999989342, 523.2161522479893847, -595.2478186815853860 ) ) ;
#11796 = EDGE_LOOP ( 'NONE', ( #10347, #15643, #1907, #13260 ) ) ;
#11797 = CARTESIAN_POINT ( 'NONE',  ( 49.99999999999999289, 515.4878487013597805, -546.7230258972048205 ) ) ;
#11798 = VECTOR ( 'NONE', #12915, 1000.000000000000000 ) ;
#11799 = EDGE_CURVE ( 'NONE', #15887, #16595, #10756, .T. ) ;
#11800 = AXIS2_PLACEMENT_3D ( 'NONE', #11036, #13869, #16361 ) ;
#11801 = VERTEX_POINT ( 'NONE', #8182 ) ;
#11802 = APPLICATION_CONTEXT ( 'automotive_design' ) ;
#11803 = EDGE_LOOP ( 'NONE', ( #2874, #9801, #13746, #2206, #4082, #12936, #7214, #2122 ) ) ;
#11804 = DIRECTION ( 'NONE',  ( 0.000000000000000000, 0.000000000000000000, 1.000000000000000000 ) ) ;
#11805 = DIRECTION ( 'NONE',  ( 1.000000000000000000, -0.000000000000000000, -0.000000000000000000 ) ) ;
#11806 = EDGE_CURVE ( 'NONE', #1759, #14371, #4739, .T. ) ;
#11807 = DIRECTION ( 'NONE',  ( 0.000000000000000000, 0.000000000000000000, 1.000000000000000000 ) ) ;
#11809 = ORIENTED_EDGE ( 'NONE', *, *, #4992, .F. ) ;
#11808 = ADVANCED_FACE ( 'NONE', ( #11016 ), #1658, .T. ) ;
#11811 = EDGE_CURVE ( 'NONE', #14719, #9593, #16084, .T. ) ;
#11810 = CARTESIAN_POINT ( 'NONE',  ( -45.00000000000000000, 515.4878487013597805, -606.7230258972047068 ) ) ;
#11812 = CARTESIAN_POINT ( 'NONE',  ( 394.0000000000001137, 339.1725919290087745, -9.945665743359786148 ) ) ;
#11813 = AXIS2_PLACEMENT_3D ( 'NONE', #1001, #5975, #2278 ) ;
#11814 = FACE_OUTER_BOUND ( 'NONE', #6588, .T. ) ;
#11815 = CARTESIAN_POINT ( 'NONE',  ( 46.99999999999988631, 493.2350855268092573, -585.2659423243250103 ) ) ;
#11816 = DIRECTION ( 'NONE',  ( -1.000000000000000000, -0.000000000000000000, -0.000000000000000000 ) ) ;
#11817 = DIRECTION ( 'NONE',  ( 0.000000000000000000, 0.000000000000000000, 1.000000000000000000 ) ) ;
#11818 = CARTESIAN_POINT ( 'NONE',  ( 18.99999999999998224, 10.00000000000000000, -35.99999999999999289 ) ) ;
#11820 = ORIENTED_EDGE ( 'NONE', *, *, #9080, .F. ) ;
#11819 = ORIENTED_EDGE ( 'NONE', *, *, #15781, .T. ) ;
#11821 = CARTESIAN_POINT ( 'NONE',  ( -3.269999999998713491, 260.4765148507195249, 287.1312267635918261 ) ) ;
#11822 = AXIS2_PLACEMENT_3D ( 'NONE', #6898, #4425, #9580 ) ;
#11823 = CARTESIAN_POINT ( 'NONE',  ( 54.99999999999999289, 460.1944820612779381, -191.6957561970704660 ) ) ;
#11824 = DIRECTION ( 'NONE',  ( -0.000000000000000000, 1.000000000000000000, -0.000000000000000000 ) ) ;
#11825 = EDGE_CURVE ( 'NONE', #12389, #21, #8323, .T. ) ;
#11826 = CARTESIAN_POINT ( 'NONE',  ( -22.99999999999999645, 68.00000000000000000, 37.00000000000002132 ) ) ;
#11827 = EDGE_CURVE ( 'NONE', #7250, #4001, #9419, .T. ) ;
#11828 = VERTEX_POINT ( 'NONE', #9387 ) ;
#11829 = EDGE_CURVE ( 'NONE', #12347, #9431, #14626, .T. ) ;
#11830 = DIRECTION ( 'NONE',  ( 0.000000000000000000, 0.000000000000000000, -1.000000000000000000 ) ) ;
#11831 = LINE ( 'NONE', #15948, #16350 ) ;
#11832 = ORIENTED_EDGE ( 'NONE', *, *, #12447, .T. ) ;
#11833 = DIRECTION ( 'NONE',  ( -0.01502673813723916056, 0.9998870921963913805, 0.000000000000000000 ) ) ;
#11834 = LINE ( 'NONE', #16895, #15791 ) ;
#11835 = EDGE_LOOP ( 'NONE', ( #12563, #14873, #9183, #15078 ) ) ;
#11836 = AXIS2_PLACEMENT_3D ( 'NONE', #6876, #12223, #9476 ) ;
#11837 = DIRECTION ( 'NONE',  ( -0.000000000000000000, -1.000000000000000000, -0.000000000000000000 ) ) ;
#11838 = LINE ( 'NONE', #11757, #6609 ) ;
#11839 = ORIENTED_EDGE ( 'NONE', *, *, #6660, .T. ) ;
#11840 = CIRCLE ( 'NONE', #10201, 4.999999999999997335 ) ;
#11841 = CARTESIAN_POINT ( 'NONE',  ( 37.50000000000000000, 196.3050121726289206, -17.00000000000000000 ) ) ;
#11842 = CONICAL_SURFACE ( 'NONE', #13224, 1.800000000000000266, 0.7853981633974524978 ) ;
#11843 = VECTOR ( 'NONE', #7951, 1000.000000000000000 ) ;
#11844 = DIRECTION ( 'NONE',  ( 0.000000000000000000, 0.000000000000000000, 1.000000000000000000 ) ) ;
#11845 = CARTESIAN_POINT ( 'NONE',  ( -46.99999999999988631, 523.2161522479888163, -489.1982331128240276 ) ) ;
#11846 = AXIS2_PLACEMENT_3D ( 'NONE', #6945, #267, #95 ) ;
#11847 = ORIENTED_EDGE ( 'NONE', *, *, #10805, .T. ) ;
#11848 = DIRECTION ( 'NONE',  ( -0.000000000000000000, -1.000000000000000000, -0.000000000000000000 ) ) ;
#11849 = PLANE ( 'NONE',  #12477 ) ;
#11850 = CARTESIAN_POINT ( 'NONE',  ( 37.00000000000000000, 68.00000000000000000, 23.00000000000001066 ) ) ;
#11851 = ORIENTED_EDGE ( 'NONE', *, *, #5790, .T. ) ;
#11852 = CARTESIAN_POINT ( 'NONE',  ( 0.000000000000000000, 309.2289037985890445, -143.5198051533984085 ) ) ;
#11853 = AXIS2_PLACEMENT_3D ( 'NONE', #13894, #15182, #11228 ) ;
#11854 = AXIS2_PLACEMENT_3D ( 'NONE', #6896, #4346, #15754 ) ;
#11855 = CARTESIAN_POINT ( 'NONE',  ( 56.72999999999999687, 264.4632308570091368, 287.5298983642207986 ) ) ;
#11856 = DIRECTION ( 'NONE',  ( 0.000000000000000000, 1.000000000000000000, -0.000000000000000000 ) ) ;
#11857 = ORIENTED_EDGE ( 'NONE', *, *, #11407, .F. ) ;
#11858 = DIRECTION ( 'NONE',  ( 1.000000000000000000, -0.000000000000000000, 0.000000000000000000 ) ) ;
#11859 = VERTEX_POINT ( 'NONE', #4493 ) ;
#11860 = VERTEX_POINT ( 'NONE', #209 ) ;
#11861 = VECTOR ( 'NONE', #1026, 1000.000000000000000 ) ;
#11862 = DIRECTION ( 'NONE',  ( 0.000000000000000000, 0.000000000000000000, -1.000000000000000000 ) ) ;
#11863 = ORIENTED_EDGE ( 'NONE', *, *, #15611, .T. ) ;
#11864 = VERTEX_POINT ( 'NONE', #2858 ) ;
#11865 = EDGE_CURVE ( 'NONE', #6948, #12012, #13350, .T. ) ;
#11866 = AXIS2_PLACEMENT_3D ( 'NONE', #14997, #16439, #3231 ) ;
#11867 = AXIS2_PLACEMENT_3D ( 'NONE', #13634, #823, #4433 ) ;
#11868 = PRESENTATION_LAYER_ASSIGNMENT (  '', '', ( #4201 ) ) ;
#11869 = VERTEX_POINT ( 'NONE', #293 ) ;
#11870 = EDGE_CURVE ( 'NONE', #14554, #9955, #8863, .T. ) ;
#11871 = ORIENTED_EDGE ( 'NONE', *, *, #8958, .T. ) ;
#11872 = DIRECTION ( 'NONE',  ( 0.000000000000000000, 0.000000000000000000, 1.000000000000000000 ) ) ;
#11873 = DIRECTION ( 'NONE',  ( 0.000000000000000000, 0.000000000000000000, -1.000000000000000000 ) ) ;
#11874 = CONICAL_SURFACE ( 'NONE', #637, 1.800000000000000266, 0.7853981633974524978 ) ;
#11875 = EDGE_LOOP ( 'NONE', ( #12846, #14598, #11424, #16756 ) ) ;
#11876 = DIRECTION ( 'NONE',  ( 0.000000000000000000, 0.000000000000000000, 1.000000000000000000 ) ) ;
#11877 = CARTESIAN_POINT ( 'NONE',  ( -36.99999999999997868, -20.00000000000000000, -22.99999999999999645 ) ) ;
#11878 = ORIENTED_EDGE ( 'NONE', *, *, #15780, .F. ) ;
#11879 = AXIS2_PLACEMENT_3D ( 'NONE', #8072, #4120, #15714 ) ;
#11880 = ADVANCED_FACE ( 'NONE', ( #2948 ), #545, .F. ) ;
#11881 = VECTOR ( 'NONE', #10056, 1000.000000000000000 ) ;
#11882 = CARTESIAN_POINT ( 'NONE',  ( -31.00000000000003197, 19.00000000000000000, -26.00000000000000355 ) ) ;
#11883 = VECTOR ( 'NONE', #9855, 1000.000000000000000 ) ;
#11884 = EDGE_LOOP ( 'NONE', ( #2219, #13501, #14277, #14892 ) ) ;
#11885 = FACE_BOUND ( 'NONE', #6450, .T. ) ;
#11886 = DIRECTION ( 'NONE',  ( 0.000000000000000000, -1.321694076934710402E-16, 1.000000000000000000 ) ) ;
#11887 = EDGE_LOOP ( 'NONE', ( #3042, #5395, #11111, #7671 ) ) ;
#11888 = DIRECTION ( 'NONE',  ( 1.000000000000000000, -0.000000000000000000, 0.000000000000000000 ) ) ;
#11889 = VERTEX_POINT ( 'NONE', #1747 ) ;
#11890 = VECTOR ( 'NONE', #1124, 1000.000000000000000 ) ;
#11891 = EDGE_CURVE ( 'NONE', #8106, #6506, #375, .T. ) ;
#11892 = DIRECTION ( 'NONE',  ( 1.000000000000000000, 0.000000000000000000, 0.000000000000000000 ) ) ;
#11893 = ORIENTED_EDGE ( 'NONE', *, *, #11193, .T. ) ;
#11894 = ORIENTED_EDGE ( 'NONE', *, *, #13227, .T. ) ;
#11895 = VECTOR ( 'NONE', #2709, 1000.000000000000000 ) ;
#11896 = AXIS2_PLACEMENT_3D ( 'NONE', #8717, #15239, #13952 ) ;
#11897 = DIRECTION ( 'NONE',  ( 0.000000000000000000, 0.000000000000000000, -1.000000000000000000 ) ) ;
#11898 = CARTESIAN_POINT ( 'NONE',  ( 31.00000000000006395, 68.00000000000000000, -22.99999999999999289 ) ) ;
#11899 = ORIENTED_EDGE ( 'NONE', *, *, #5247, .F. ) ;
#11900 = DIRECTION ( 'NONE',  ( -0.000000000000000000, -1.000000000000000000, -0.000000000000000000 ) ) ;
#11901 = CIRCLE ( 'NONE', #16293, 13.69540538389601991 ) ;
#11902 = DIRECTION ( 'NONE',  ( -0.000000000000000000, 1.000000000000000000, -0.000000000000000000 ) ) ;
#11903 = AXIS2_PLACEMENT_3D ( 'NONE', #16567, #12537, #857 ) ;
#11904 = EDGE_CURVE ( 'NONE', #12818, #6752, #5690, .T. ) ;
#11905 = CARTESIAN_POINT ( 'NONE',  ( -34.99999999999996447, 8.000000000000000000, 40.00000000000000711 ) ) ;
#11906 = CARTESIAN_POINT ( 'NONE',  ( 55.99999999999989342, 559.9933750504617365, -546.7230258972048205 ) ) ;
#11907 = CARTESIAN_POINT ( 'NONE',  ( 394.0000000000001137, 234.3157724647196289, -17.15546574335979813 ) ) ;
#11908 = CIRCLE ( 'NONE', #8901, 13.69540538389601991 ) ;
#11909 = VECTOR ( 'NONE', #11531, 1000.000000000000000 ) ;
#11910 = CARTESIAN_POINT ( 'NONE',  ( 17.00000000000000711, 380.0000000000000000, -17.00000000000000355 ) ) ;
#11911 = AXIS2_PLACEMENT_3D ( 'NONE', #9984, #4408, #8442 ) ;
#11912 =( LENGTH_UNIT ( ) NAMED_UNIT ( * ) SI_UNIT ( .MILLI., .METRE. ) );
#11914 = ORIENTED_EDGE ( 'NONE', *, *, #14333, .F. ) ;
#11913 = ORIENTED_EDGE ( 'NONE', *, *, #7944, .F. ) ;
#11915 = EDGE_CURVE ( 'NONE', #13073, #11007, #12442, .T. ) ;
#11916 = CARTESIAN_POINT ( 'NONE',  ( -39.99999999999999289, 11.00000000000000000, 34.99999999999997868 ) ) ;
#11917 = EDGE_CURVE ( 'NONE', #14972, #748, #6953, .T. ) ;
#11918 = VECTOR ( 'NONE', #3023, 1000.000000000000000 ) ;
#11919 = CARTESIAN_POINT ( 'NONE',  ( 0.03302700000112353956, 285.5316255717817171, 37.50583589681555452 ) ) ;
#11920 = DIRECTION ( 'NONE',  ( 3.854941057726247958E-16, -0.000000000000000000, 1.000000000000000000 ) ) ;
#11921 = ORIENTED_EDGE ( 'NONE', *, *, #5085, .F. ) ;
#11922 = AXIS2_PLACEMENT_3D ( 'NONE', #15642, #3801, #6606 ) ;
#11923 = AXIS2_PLACEMENT_3D ( 'NONE', #14516, #9109, #10828 ) ;
#11924 = CARTESIAN_POINT ( 'NONE',  ( 2.799999999999999822, 0.000000000000000000, 0.000000000000000000 ) ) ;
#11925 = DIRECTION ( 'NONE',  ( 0.000000000000000000, 1.000000000000000000, 0.000000000000000000 ) ) ;
#11927 = EDGE_CURVE ( 'NONE', #11171, #1082, #13820, .T. ) ;
#11926 = ORIENTED_EDGE ( 'NONE', *, *, #3121, .F. ) ;
#11928 = CARTESIAN_POINT ( 'NONE',  ( 414.7091847417151484, 350.3558646104334571, 0.000000000000000000 ) ) ;
#11929 = VECTOR ( 'NONE', #9706, 1000.000000000000000 ) ;
#11930 = DIRECTION ( 'NONE',  ( -1.000000000000000000, -0.000000000000000000, -0.000000000000000000 ) ) ;
#11931 = CARTESIAN_POINT ( 'NONE',  ( 46.99999999999988631, 493.2350855268086320, -512.8755148539809170 ) ) ;
#11932 = CARTESIAN_POINT ( 'NONE',  ( 25.99999999999997868, 10.00000000000000000, 40.00000000000000711 ) ) ;
#11933 = CYLINDRICAL_SURFACE ( 'NONE', #2387, 13.69540538389596485 ) ;
#11934 = DIRECTION ( 'NONE',  ( 1.000000000000000000, 0.000000000000000000, 0.000000000000000000 ) ) ;
#11935 = VERTEX_POINT ( 'NONE', #12557 ) ;
#11936 = ADVANCED_FACE ( 'NONE', ( #7131 ), #4820, .T. ) ;
#11937 = EDGE_CURVE ( 'NONE', #16470, #10513, #8612, .T. ) ;
#11938 = EDGE_CURVE ( 'NONE', #12512, #8036, #15307, .T. ) ;
#11939 = CARTESIAN_POINT ( 'NONE',  ( 31.00000000000001776, 10.00000000000000000, -25.99999999999999645 ) ) ;
#11940 = PRODUCT_DEFINITION_FORMATION_WITH_SPECIFIED_SOURCE ( 'ANY', '', #1513, .NOT_KNOWN. ) ;
#11941 = EDGE_CURVE ( 'NONE', #15487, #5457, #9820, .T. ) ;
#11942 = DIRECTION ( 'NONE',  ( 0.000000000000000000, 0.000000000000000000, -1.000000000000000000 ) ) ;
#11943 = AXIS2_PLACEMENT_3D ( 'NONE', #9688, #659, #10884 ) ;
#11944 = CARTESIAN_POINT ( 'NONE',  ( 31.81980515339464333, 8.000000000000000000, 31.81980515339463622 ) ) ;
#11945 = ORIENTED_EDGE ( 'NONE', *, *, #15092, .F. ) ;
#11946 = DIRECTION ( 'NONE',  ( 0.000000000000000000, -0.000000000000000000, -1.000000000000000000 ) ) ;
#11947 = CARTESIAN_POINT ( 'NONE',  ( 3.500000000000000000, 0.000000000000000000, 0.000000000000000000 ) ) ;
#11948 = CARTESIAN_POINT ( 'NONE',  ( 55.99999999999989342, 549.5810598491749488, -589.0260321808809749 ) ) ;
#11949 = ORIENTED_EDGE ( 'NONE', *, *, #2828, .T. ) ;
#11950 = DIRECTION ( 'NONE',  ( 1.000000000000000000, 0.000000000000000000, -0.000000000000000000 ) ) ;
#11951 = FACE_OUTER_BOUND ( 'NONE', #16940, .T. ) ;
#11952 = CARTESIAN_POINT ( 'NONE',  ( 31.00000000000004263, 0.000000000000000000, -25.99999999999999645 ) ) ;
#11953 = ORIENTED_EDGE ( 'NONE', *, *, #6439, .T. ) ;
#11954 = AXIS2_PLACEMENT_3D ( 'NONE', #2960, #13273, #4253 ) ;
#11955 = CARTESIAN_POINT ( 'NONE',  ( -37.00000000000000000, 68.00000000000000000, 23.00000000000000355 ) ) ;
#11956 = VERTEX_POINT ( 'NONE', #7463 ) ;
#11957 = ORIENTED_EDGE ( 'NONE', *, *, #1566, .T. ) ;
#11958 = DIRECTION ( 'NONE',  ( 0.000000000000000000, 0.000000000000000000, 1.000000000000000000 ) ) ;
#11959 = EDGE_CURVE ( 'NONE', #1481, #10388, #12994, .T. ) ;
#11960 = VERTEX_POINT ( 'NONE', #13851 ) ;
#11961 = SHAPE_DEFINITION_REPRESENTATION ( #10995, #1883 ) ;
#11962 = ORIENTED_EDGE ( 'NONE', *, *, #12164, .F. ) ;
#11963 = AXIS2_PLACEMENT_3D ( 'NONE', #6711, #15785, #9091 ) ;
#11964 = ORIENTED_EDGE ( 'NONE', *, *, #10449, .F. ) ;
#11965 = AXIS2_PLACEMENT_3D ( 'NONE', #2214, #12702, #16319 ) ;
#11966 = CARTESIAN_POINT ( 'NONE',  ( 25.99999999999997868, 10.00000000000000000, 40.00000000000000711 ) ) ;
#11967 = DIRECTION ( 'NONE',  ( 1.000000000000000000, 0.000000000000000000, 0.000000000000000000 ) ) ;
#11968 = EDGE_LOOP ( 'NONE', ( #14200, #14212, #16777, #9436 ) ) ;
#11969 = DIRECTION ( 'NONE',  ( 0.000000000000000000, 0.000000000000000000, -1.000000000000000000 ) ) ;
#11970 = EDGE_CURVE ( 'NONE', #2956, #15552, #4901, .T. ) ;
#11971 = DIRECTION ( 'NONE',  ( -1.000000000000000000, -0.000000000000000000, -0.000000000000000000 ) ) ;
#11972 = ORIENTED_EDGE ( 'NONE', *, *, #13593, .T. ) ;
#11973 = CARTESIAN_POINT ( 'NONE',  ( 35.99999999999999289, 6.000000000000000000, 21.99999999999999645 ) ) ;
#11974 = EDGE_LOOP ( 'NONE', ( #3208, #7142, #2163, #11349 ) ) ;
#11975 = CARTESIAN_POINT ( 'NONE',  ( 23.00000000000000711, 68.00000000000000000, -31.00000000000002487 ) ) ;
#11976 = CARTESIAN_POINT ( 'NONE',  ( 26.00000000000000000, 19.00000000000000000, 40.00000000000001421 ) ) ;
#11977 = VERTEX_POINT ( 'NONE', #797 ) ;
#11978 = VECTOR ( 'NONE', #15522, 1000.000000000000000 ) ;
#11979 = AXIS2_PLACEMENT_3D ( 'NONE', #2053, #15201, #7283 ) ;
#11980 = CARTESIAN_POINT ( 'NONE',  ( 0.000000000000000000, 38.00000000000000711, -5.741599279633704455E-16 ) ) ;
#11981 = ORIENTED_EDGE ( 'NONE', *, *, #11385, .F. ) ;
#11982 = SHAPE_REPRESENTATION_RELATIONSHIP ( 'NONE' , 'NONE' ,  #16471, #6453 ) ;
#11983 = LINE ( 'NONE', #1503, #178 ) ;
#11984 = ORIENTED_EDGE ( 'NONE', *, *, #5056, .F. ) ;
#11985 = ORIENTED_EDGE ( 'NONE', *, *, #10244, .F. ) ;
#11986 = DIRECTION ( 'NONE',  ( -0.000000000000000000, -1.000000000000000000, -0.000000000000000000 ) ) ;
#11987 = FACE_OUTER_BOUND ( 'NONE', #14138, .T. ) ;
#11988 = CARTESIAN_POINT ( 'NONE',  ( -55.99999999999988631, 658.4713480608917280, -425.4301204538002139 ) ) ;
#11989 = CIRCLE ( 'NONE', #5949, 15.25000000000000000 ) ;
#11990 = ORIENTED_EDGE ( 'NONE', *, *, #16335, .T. ) ;
#11991 = AXIS2_PLACEMENT_3D ( 'NONE', #16545, #9783, #16208 ) ;
#11992 = CARTESIAN_POINT ( 'NONE',  ( 55.99999999999989342, 493.2350855268086320, -512.8755148539809170 ) ) ;
#11993 = DIRECTION ( 'NONE',  ( 1.000000000000000000, -0.000000000000000000, 0.000000000000000000 ) ) ;
#11994 = LINE ( 'NONE', #12165, #10676 ) ;
#11995 = DIRECTION ( 'NONE',  ( -1.000000000000000000, -0.000000000000000000, -0.000000000000000000 ) ) ;
#11996 = CARTESIAN_POINT ( 'NONE',  ( 0.000000000000000000, 339.1725919290084335, -111.4188657433597456 ) ) ;
#11997 = DIRECTION ( 'NONE',  ( -0.000000000000000000, -1.000000000000000000, -0.000000000000000000 ) ) ;
#11998 = DIRECTION ( 'NONE',  ( 0.000000000000000000, 0.000000000000000000, 1.000000000000000000 ) ) ;
#12000 = ORIENTED_EDGE ( 'NONE', *, *, #4654, .F. ) ;
#11999 = VERTEX_POINT ( 'NONE', #8778 ) ;
#12001 = VECTOR ( 'NONE', #215, 1000.000000000000000 ) ;
#12002 = DIRECTION ( 'NONE',  ( 0.000000000000000000, 0.000000000000000000, 1.000000000000000000 ) ) ;
#12003 = DIRECTION ( 'NONE',  ( -1.000000000000000000, -0.000000000000000000, -0.000000000000000000 ) ) ;
#12004 = ADVANCED_FACE ( 'NONE', ( #964 ), #3371, .T. ) ;
#12005 = LINE ( 'NONE', #2636, #14829 ) ;
#12006 = PLANE ( 'NONE',  #6104 ) ;
#12007 = VERTEX_POINT ( 'NONE', #3287 ) ;
#12008 = DIRECTION ( 'NONE',  ( 0.000000000000000000, 0.000000000000000000, 1.000000000000000000 ) ) ;
#12009 = VECTOR ( 'NONE', #15019, 1000.000000000000000 ) ;
#12010 = EDGE_CURVE ( 'NONE', #2523, #1746, #7308, .T. ) ;
#12011 = CARTESIAN_POINT ( 'NONE',  ( 25.99999999999996092, 3.000000000000000000, -31.00000000000003197 ) ) ;
#12012 = VERTEX_POINT ( 'NONE', #1988 ) ;
#12013 = LINE ( 'NONE', #16131, #5203 ) ;
#12014 = FACE_OUTER_BOUND ( 'NONE', #13677, .T. ) ;
#12015 = DIRECTION ( 'NONE',  ( 1.000000000000000000, -0.000000000000000000, -0.000000000000000000 ) ) ;
#12016 = DIRECTION ( 'NONE',  ( -3.854941057726249437E-16, 0.000000000000000000, -1.000000000000000000 ) ) ;
#12017 = SURFACE_STYLE_USAGE ( .BOTH. , #8060 ) ;
#12018 = CARTESIAN_POINT ( 'NONE',  ( -32.00000000000000711, 6.000000000000000000, -22.00000000000000355 ) ) ;
#12019 = ORIENTED_EDGE ( 'NONE', *, *, #1652, .F. ) ;
#12020 = ADVANCED_BREP_SHAPE_REPRESENTATION ( '', ( #14587, #1488 ), #16030 ) ;
#12021 = CARTESIAN_POINT ( 'NONE',  ( -31.81980515339462912, 11.00000000000000000, 28.51980515339464617 ) ) ;
#12022 = CYLINDRICAL_SURFACE ( 'NONE', #10965, 60.00000000000000000 ) ;
#12023 = EDGE_CURVE ( 'NONE', #8165, #4736, #2077, .T. ) ;
#12024 = CARTESIAN_POINT ( 'NONE',  ( 449.9999999999998295, 106.2500000000000142, 0.000000000000000000 ) ) ;
#12025 = VERTEX_POINT ( 'NONE', #874 ) ;
#12026 = DIRECTION ( 'NONE',  ( 0.000000000000000000, 0.000000000000000000, -1.000000000000000000 ) ) ;
#12027 = UNCERTAINTY_MEASURE_WITH_UNIT (LENGTH_MEASURE( 1.000000000000000082E-05 ), #12468, 'distance_accuracy_value', 'NONE');
#12028 = EDGE_CURVE ( 'NONE', #4908, #4138, #2283, .T. ) ;
#12029 = DIRECTION ( 'NONE',  ( 1.000000000000000000, 2.935544750463131859E-15, 4.905671055753177464E-32 ) ) ;
#12030 = EDGE_CURVE ( 'NONE', #8474, #4609, #15125, .T. ) ;
#12031 = ADVANCED_FACE ( 'NONE', ( #9987 ), #13936, .F. ) ;
#12032 = PLANE ( 'NONE',  #10311 ) ;
#12033 = ORIENTED_EDGE ( 'NONE', *, *, #1817, .F. ) ;
#12034 = DIRECTION ( 'NONE',  ( 0.000000000000000000, 0.000000000000000000, 1.000000000000000000 ) ) ;
#12035 = ADVANCED_FACE ( 'NONE', ( #12636 ), #6097, .T. ) ;
#12036 = PLANE ( 'NONE',  #10643 ) ;
#12037 = DIRECTION ( 'NONE',  ( 0.000000000000000000, -0.6930515690182840194, -0.7208880098054721852 ) ) ;
#12038 = ORIENTED_EDGE ( 'NONE', *, *, #5777, .T. ) ;
#12039 = CIRCLE ( 'NONE', #15047, 22.75209553982836397 ) ;
#12040 = CARTESIAN_POINT ( 'NONE',  ( 25.99999999999998224, 8.000000000000000000, -32.99999999999999289 ) ) ;
#12041 = ORIENTED_EDGE ( 'NONE', *, *, #9634, .F. ) ;
#12042 = ORIENTED_EDGE ( 'NONE', *, *, #485, .T. ) ;
#12043 = CARTESIAN_POINT ( 'NONE',  ( -55.99999999999989342, 473.6663340069158039, -561.9448123979092315 ) ) ;
#12044 = VERTEX_POINT ( 'NONE', #13147 ) ;
#12045 = ORIENTED_EDGE ( 'NONE', *, *, #16332, .F. ) ;
#12046 = EDGE_LOOP ( 'NONE', ( #12683, #16441, #8740, #14149 ) ) ;
#12047 = DIRECTION ( 'NONE',  ( 0.000000000000000000, 0.000000000000000000, 1.000000000000000000 ) ) ;
#12048 = EDGE_CURVE ( 'NONE', #16344, #12347, #14366, .T. ) ;
#12049 = LINE ( 'NONE', #9562, #4764 ) ;
#12050 = ADVANCED_FACE ( 'NONE', ( #7811 ), #13071, .T. ) ;
#12051 = VERTEX_POINT ( 'NONE', #12979 ) ;
#12052 = DIRECTION ( 'NONE',  ( 0.000000000000000000, 0.000000000000000000, 1.000000000000000000 ) ) ;
#12053 = EDGE_CURVE ( 'NONE', #1073, #11097, #15731, .T. ) ;
#12054 = DIRECTION ( 'NONE',  ( 0.000000000000000000, 0.000000000000000000, -1.000000000000000000 ) ) ;
#12055 = VERTEX_POINT ( 'NONE', #12813 ) ;
#12056 = AXIS2_PLACEMENT_3D ( 'NONE', #14567, #4171, #12075 ) ;
#12057 =( LENGTH_UNIT ( ) NAMED_UNIT ( * ) SI_UNIT ( .MILLI., .METRE. ) );
#12058 = ORIENTED_EDGE ( 'NONE', *, *, #16143, .T. ) ;
#12059 = CARTESIAN_POINT ( 'NONE',  ( 0.000000000000000000, 0.000000000000000000, 0.000000000000000000 ) ) ;
#12060 = CARTESIAN_POINT ( 'NONE',  ( 0.000000000000000000, 341.5974953295086038, -15.94751227074151956 ) ) ;
#12061 = EDGE_LOOP ( 'NONE', ( #3240, #5256, #10251, #5070 ) ) ;
#12062 = CARTESIAN_POINT ( 'NONE',  ( 44.68009836720081296, 275.4439001176564830, -17.00000000000000000 ) ) ;
#12063 = ORIENTED_EDGE ( 'NONE', *, *, #13510, .T. ) ;
#12064 = DIRECTION ( 'NONE',  ( -3.553708640349240840E-17, 1.000000000000000000, 4.699395265751666769E-17 ) ) ;
#12065 = DIRECTION ( 'NONE',  ( -0.000000000000000000, -1.000000000000000000, -0.000000000000000000 ) ) ;
#12066 = ORIENTED_EDGE ( 'NONE', *, *, #6023, .T. ) ;
#12067 = TOROIDAL_SURFACE ( 'NONE', #6273, 4.695405383895982609, 9.000000000000000000 ) ;
#12068 = EDGE_LOOP ( 'NONE', ( #3464, #10511, #1706, #4257 ) ) ;
#12069 = DIRECTION ( 'NONE',  ( -1.000000000000000000, 0.000000000000000000, 0.000000000000000000 ) ) ;
#12070 = LINE ( 'NONE', #5445, #3882 ) ;
#12071 = DIRECTION ( 'NONE',  ( 1.000000000000000000, 0.000000000000000000, 0.000000000000000000 ) ) ;
#12072 = DIRECTION ( 'NONE',  ( 1.000000000000000000, 0.000000000000000000, 0.000000000000000000 ) ) ;
#12073 = PRODUCT ( 'Part2', 'Part2', '', ( #16582 ) ) ;
#12074 = LINE ( 'NONE', #6815, #16291 ) ;
#12075 = DIRECTION ( 'NONE',  ( 0.000000000000000000, 0.000000000000000000, 1.000000000000000000 ) ) ;
#12076 = DIRECTION ( 'NONE',  ( -1.000000000000000000, -0.000000000000000000, 0.000000000000000000 ) ) ;
#12077 = CARTESIAN_POINT ( 'NONE',  ( 449.9999999999998295, 75.00000000000001421, 3.000000000000000000 ) ) ;
#12078 = CARTESIAN_POINT ( 'NONE',  ( 0.000000000000000000, -0.000000000000000000, -206.3519347178565795 ) ) ;
#12079 = VECTOR ( 'NONE', #16712, 1000.000000000000000 ) ;
#12080 = VECTOR ( 'NONE', #7535, 1000.000000000000227 ) ;
#12081 = FACE_OUTER_BOUND ( 'NONE', #13601, .T. ) ;
#12082 = CARTESIAN_POINT ( 'NONE',  ( -19.00000000000001776, 10.00000000000000000, 36.00000000000000711 ) ) ;
#12084 = ORIENTED_EDGE ( 'NONE', *, *, #11216, .T. ) ;
#12083 = ORIENTED_EDGE ( 'NONE', *, *, #6766, .F. ) ;
#12085 = CARTESIAN_POINT ( 'NONE',  ( -34.99999999999999289, 0.000000000000000000, 35.00000000000000711 ) ) ;
#12086 = CARTESIAN_POINT ( 'NONE',  ( -0.3206782292933404999, 289.3845136302657579, 37.58913636098598232 ) ) ;
#12087 = DIRECTION ( 'NONE',  ( -1.000000000000000000, -0.000000000000000000, -0.000000000000000000 ) ) ;
#12088 = CARTESIAN_POINT ( 'NONE',  ( 25.99999999999998224, 10.00000000000000000, -31.00000000000003197 ) ) ;
#12089 = AXIS2_PLACEMENT_3D ( 'NONE', #6208, #10177, #15748 ) ;
#12090 = VERTEX_POINT ( 'NONE', #10231 ) ;
#12091 = LINE ( 'NONE', #331, #12964 ) ;
#12092 = CARTESIAN_POINT ( 'NONE',  ( -40.00000000000000711, 10.00000000000000000, -19.00000000000000355 ) ) ;
#12093 = ORIENTED_EDGE ( 'NONE', *, *, #1208, .T. ) ;
#12094 = CARTESIAN_POINT ( 'NONE',  ( -22.99999999999999645, 68.00000000000000000, 37.00000000000002132 ) ) ;
#12095 = CARTESIAN_POINT ( 'NONE',  ( 6.299999999999999822, 0.000000000000000000, 0.000000000000000000 ) ) ;
#12096 = DIRECTION ( 'NONE',  ( 0.000000000000000000, -1.000000000000000000, -0.000000000000000000 ) ) ;
#12097 = ORIENTED_EDGE ( 'NONE', *, *, #7255, .T. ) ;
#12098 = ADVANCED_FACE ( 'NONE', ( #9113 ), #2663, .T. ) ;
#12099 = CARTESIAN_POINT ( 'NONE',  ( 414.7091847417151484, 350.3558646104334571, -6.736600000000000144 ) ) ;
#12100 = CARTESIAN_POINT ( 'NONE',  ( -7.005190481990339112E-15, 37.39913938097243573, -5.741599279633704455E-16 ) ) ;
#12101 = CARTESIAN_POINT ( 'NONE',  ( -31.00000000000005329, 10.00000000000000000, 26.00000000000000000 ) ) ;
#12102 = EDGE_LOOP ( 'NONE', ( #10602, #4311, #16206, #14378 ) ) ;
#12103 = B_SPLINE_CURVE_WITH_KNOTS ( 'NONE', 3,
 ( #812, #8455, #11272, #9669, #1919, #3385, #6028, #5955, #12401, #15143, #11197, #6989, #4424, #3300, #560, #16430, #13861, #480 ),
 .UNSPECIFIED., .F., .F.,
 ( 4, 2, 2, 2, 2, 2, 2, 2, 4 ),
 ( 0.004721323624227206743, 0.005310725018217476653, 0.005900126412207745696, 0.006489527806198015607, 0.007078929200188285517, 0.007668330594178554560, 0.008257731988168825338, 0.008847133382159092646, 0.009436534776149363424 ),
 .UNSPECIFIED. ) ;
#12104 = CIRCLE ( 'NONE', #11258, 9.000000000000007105 ) ;
#12105 = DIRECTION ( 'NONE',  ( -1.000000000000000000, 0.000000000000000000, 0.000000000000000000 ) ) ;
#12106 = EDGE_CURVE ( 'NONE', #11696, #12951, #10569, .T. ) ;
#12107 = DIRECTION ( 'NONE',  ( 6.123031769111888756E-17, 0.000000000000000000, 1.000000000000000000 ) ) ;
#12108 = CARTESIAN_POINT ( 'NONE',  ( 40.00000000000000711, 19.00000000000000000, 25.99999999999999645 ) ) ;
#12109 = EDGE_LOOP ( 'NONE', ( #7335, #11984, #826, #3541 ) ) ;
#12110 = CARTESIAN_POINT ( 'NONE',  ( 49.99999999999999289, 515.4878487013597805, -546.7230258972048205 ) ) ;
#12111 = DIRECTION ( 'NONE',  ( 0.000000000000000000, 0.000000000000000000, 1.000000000000000000 ) ) ;
#12112 = AXIS2_PLACEMENT_3D ( 'NONE', #16103, #6812, #12322 ) ;
#12113 = CARTESIAN_POINT ( 'NONE',  ( 5.941205806953520074, 0.000000000000000000, 0.000000000000000000 ) ) ;
#12114 = ORIENTED_EDGE ( 'NONE', *, *, #6816, .F. ) ;
#12115 = DIRECTION ( 'NONE',  ( 0.000000000000000000, 0.6427876096865285938, 0.7660444431189872283 ) ) ;
#12116 = DIRECTION ( 'NONE',  ( 0.000000000000000000, 0.000000000000000000, 1.000000000000000000 ) ) ;
#12117 = DIRECTION ( 'NONE',  ( -7.709882115452498874E-16, 0.000000000000000000, -1.000000000000000000 ) ) ;
#12118 = ORIENTED_EDGE ( 'NONE', *, *, #2516, .T. ) ;
#12119 = ADVANCED_FACE ( 'NONE', ( #1295 ), #5068, .F. ) ;
#12120 = SURFACE_STYLE_FILL_AREA ( #4396 ) ;
#12121 = ADVANCED_FACE ( 'NONE', ( #10480 ), #7496, .T. ) ;
#12122 = ORIENTED_EDGE ( 'NONE', *, *, #12641, .T. ) ;
#12123 = VERTEX_POINT ( 'NONE', #3966 ) ;
#12124 = CYLINDRICAL_SURFACE ( 'NONE', #125, 5.000000000000004441 ) ;
#12125 = ORIENTED_EDGE ( 'NONE', *, *, #231, .F. ) ;
#12126 = EDGE_CURVE ( 'NONE', #7102, #13859, #9206, .T. ) ;
#12127 = DIRECTION ( 'NONE',  ( 1.000000000000000000, 0.000000000000000000, 0.000000000000000000 ) ) ;
#12128 = CIRCLE ( 'NONE', #11836, 15.25000000000000000 ) ;
#12129 = EDGE_CURVE ( 'NONE', #3814, #6268, #14442, .T. ) ;
#12130 = ADVANCED_FACE ( 'NONE', ( #11688 ), #8337, .F. ) ;
#12131 = EDGE_LOOP ( 'NONE', ( #1499, #4379, #5172, #8665, #5845, #3138, #1306, #15690 ) ) ;
#12132 = VECTOR ( 'NONE', #5365, 1000.000000000000000 ) ;
#12133 = ORIENTED_EDGE ( 'NONE', *, *, #3362, .T. ) ;
#12134 = DIRECTION ( 'NONE',  ( -1.000000000000000000, -0.000000000000000000, -0.000000000000000000 ) ) ;
#12135 = CARTESIAN_POINT ( 'NONE',  ( -55.99999999999989342, 559.9933750504617365, -542.0276205133087615 ) ) ;
#12136 = ORIENTED_EDGE ( 'NONE', *, *, #2364, .F. ) ;
#12137 = DIRECTION ( 'NONE',  ( -2.556703065963791256E-16, 1.000000000000000000, 0.000000000000000000 ) ) ;
#12138 = AXIS2_PLACEMENT_3D ( 'NONE', #12689, #928, #3676 ) ;
#12139 = FACE_OUTER_BOUND ( 'NONE', #13987, .T. ) ;
#12140 = VERTEX_POINT ( 'NONE', #11852 ) ;
#12141 = EDGE_CURVE ( 'NONE', #13213, #10404, #5325, .T. ) ;
#12142 = CARTESIAN_POINT ( 'NONE',  ( -23.00000000000003197, 3.000000000000000000, 34.00000000000000711 ) ) ;
#12143 = EDGE_LOOP ( 'NONE', ( #6895, #13050, #8481, #2422 ) ) ;
#12144 = FACE_OUTER_BOUND ( 'NONE', #1221, .T. ) ;
#12145 = LINE ( 'NONE', #11792, #4734 ) ;
#12146 = VERTEX_POINT ( 'NONE', #3711 ) ;
#12147 = AXIS2_PLACEMENT_3D ( 'NONE', #13823, #13985, #936 ) ;
#12148 = DIRECTION ( 'NONE',  ( 1.000000000000000000, 2.935544750463131859E-15, 4.954244443042633456E-32 ) ) ;
#12149 = ORIENTED_EDGE ( 'NONE', *, *, #3605, .F. ) ;
#12150 = EDGE_CURVE ( 'NONE', #16617, #3282, #4756, .T. ) ;
#12151 = EDGE_CURVE ( 'NONE', #13257, #7500, #7637, .T. ) ;
#12152 = CARTESIAN_POINT ( 'NONE',  ( -31.00000000000002842, 68.00000000000000000, -25.99999999999999645 ) ) ;
#12153 = EDGE_CURVE ( 'NONE', #9431, #11779, #9159, .T. ) ;
#12154 = ORIENTED_EDGE ( 'NONE', *, *, #4064, .T. ) ;
#12155 = AXIS2_PLACEMENT_3D ( 'NONE', #7532, #15861, #1613 ) ;
#12156 = VERTEX_POINT ( 'NONE', #10400 ) ;
#12157 = LINE ( 'NONE', #10777, #12680 ) ;
#12158 = CYLINDRICAL_SURFACE ( 'NONE', #9362, 13.69540538389601991 ) ;
#12159 = CARTESIAN_POINT ( 'NONE',  ( 394.0000000000001137, 339.1725919290084335, -111.4188657433597456 ) ) ;
#12160 = CARTESIAN_POINT ( 'NONE',  ( -22.00000000000001776, 6.000000000000000000, 32.00000000000000711 ) ) ;
#12161 = AXIS2_PLACEMENT_3D ( 'NONE', #4891, #15456, #9752 ) ;
#12162 = AXIS2_PLACEMENT_3D ( 'NONE', #7164, #11389, #2194 ) ;
#12163 = FACE_OUTER_BOUND ( 'NONE', #3848, .T. ) ;
#12164 = EDGE_CURVE ( 'NONE', #1188, #5722, #14926, .T. ) ;
#12165 = CARTESIAN_POINT ( 'NONE',  ( 31.00000000000006750, 8.000000000000000000, -21.00000000000000355 ) ) ;
#12166 = CARTESIAN_POINT ( 'NONE',  ( -30.99999999999999645, 68.00000000000000000, -30.99999999999999289 ) ) ;
#12167 = LINE ( 'NONE', #5370, #15008 ) ;
#12168 = DIRECTION ( 'NONE',  ( -3.854941057726249437E-16, 0.000000000000000000, -1.000000000000000000 ) ) ;
#12169 = CIRCLE ( 'NONE', #372, 2.999999999999995559 ) ;
#12170 = CYLINDRICAL_SURFACE ( 'NONE', #5303, 13.69540538389601991 ) ;
#12171 = CARTESIAN_POINT ( 'NONE',  ( 25.99999999999999645, 0.000000000000000000, 40.00000000000002132 ) ) ;
#12173 = EDGE_LOOP ( 'NONE', ( #10843, #10807, #340, #4480 ) ) ;
#12172 = ORIENTED_EDGE ( 'NONE', *, *, #4789, .T. ) ;
#12174 = AXIS2_PLACEMENT_3D ( 'NONE', #9483, #1753, #2772 ) ;
#12175 = DIRECTION ( 'NONE',  ( -1.000000000000000000, 0.000000000000000000, -0.000000000000000000 ) ) ;
#12176 = AXIS2_PLACEMENT_3D ( 'NONE', #2790, #5627, #4169 ) ;
#12177 = AXIS2_PLACEMENT_3D ( 'NONE', #8116, #5363, #14562 ) ;
#12178 = CARTESIAN_POINT ( 'NONE',  ( 31.99999999999998579, 6.000000000000000000, 21.99999999999999645 ) ) ;
#12179 = FACE_OUTER_BOUND ( 'NONE', #712, .T. ) ;
#12180 = DIRECTION ( 'NONE',  ( 0.000000000000000000, -1.000000000000000000, 0.000000000000000000 ) ) ;
#12181 = VECTOR ( 'NONE', #16748, 1000.000000000000000 ) ;
#12182 = ORIENTED_EDGE ( 'NONE', *, *, #8896, .F. ) ;
#12183 = DIRECTION ( 'NONE',  ( -0.000000000000000000, -1.000000000000000000, 0.000000000000000000 ) ) ;
#12184 =( GEOMETRIC_REPRESENTATION_CONTEXT ( 3 ) GLOBAL_UNCERTAINTY_ASSIGNED_CONTEXT ( ( #14145 ) ) GLOBAL_UNIT_ASSIGNED_CONTEXT ( ( #303, #4341, #10684 ) ) REPRESENTATION_CONTEXT ( 'NONE', 'WORKASPACE' ) );
#12185 = FACE_BOUND ( 'NONE', #5698, .T. ) ;
#12186 = EDGE_LOOP ( 'NONE', ( #16086, #2593, #13712, #15103 ) ) ;
#12187 = LINE ( 'NONE', #6836, #1097 ) ;
#12188 = CIRCLE ( 'NONE', #4241, 13.69540538389601991 ) ;
#12189 = ADVANCED_FACE ( 'NONE', ( #4124, #4313 ), #1467, .F. ) ;
#12190 = CARTESIAN_POINT ( 'NONE',  ( 1.050000000000000044, 17.52499999999999858, 0.000000000000000000 ) ) ;
#12191 = FACE_BOUND ( 'NONE', #10776, .T. ) ;
#12192 = CARTESIAN_POINT ( 'NONE',  ( -25.99999999999999645, 68.00000000000000000, -31.00000000000003197 ) ) ;
#12193 = DIRECTION ( 'NONE',  ( 1.000000000000000000, 0.000000000000000000, 0.000000000000000000 ) ) ;
#12194 = ORIENTED_EDGE ( 'NONE', *, *, #10343, .T. ) ;
#12195 = AXIS2_PLACEMENT_3D ( 'NONE', #9803, #2216, #12452 ) ;
#12196 = EDGE_CURVE ( 'NONE', #793, #6189, #1471, .T. ) ;
#12197 = DIRECTION ( 'NONE',  ( 0.000000000000000000, 0.000000000000000000, 1.000000000000000000 ) ) ;
#12198 = CARTESIAN_POINT ( 'NONE',  ( -55.99999999999989342, 473.6663340069158039, -557.2494070140132862 ) ) ;
#12199 = AXIS2_PLACEMENT_3D ( 'NONE', #16456, #9943, #917 ) ;
#12200 = SURFACE_STYLE_FILL_AREA ( #16060 ) ;
#12201 = ORIENTED_EDGE ( 'NONE', *, *, #1634, .F. ) ;
#12202 = PRODUCT_DEFINITION ( 'UNKNOWN', '', #13014, #12592 ) ;
#12203 = AXIS2_PLACEMENT_3D ( 'NONE', #14961, #16242, #16485 ) ;
#12204 = FACE_OUTER_BOUND ( 'NONE', #15413, .T. ) ;
#12205 = UNCERTAINTY_MEASURE_WITH_UNIT (LENGTH_MEASURE( 1.000000000000000082E-05 ), #3381, 'distance_accuracy_value', 'NONE');
#12206 = CARTESIAN_POINT ( 'NONE',  ( 44.68009836720079875, 352.3758082234937206, -75.00000000000000000 ) ) ;
#12207 = ORIENTED_EDGE ( 'NONE', *, *, #7486, .T. ) ;
#12208 = CARTESIAN_POINT ( 'NONE',  ( 0.000000000000000000, 239.4632308570078294, 56.73739990498292940 ) ) ;
#12209 = CARTESIAN_POINT ( 'NONE',  ( 55.99999999999989342, 473.6663340069158039, -566.6402177818052905 ) ) ;
#12210 = DIRECTION ( 'NONE',  ( -1.000000000000000000, -0.000000000000000000, -0.000000000000000000 ) ) ;
#12211 = ORIENTED_EDGE ( 'NONE', *, *, #3072, .T. ) ;
#12212 = EDGE_CURVE ( 'NONE', #9007, #7500, #9282, .T. ) ;
#12213 = CARTESIAN_POINT ( 'NONE',  ( 26.00000000000000355, 11.00000000000000000, -40.00000000000000711 ) ) ;
#12214 = VERTEX_POINT ( 'NONE', #9547 ) ;
#12215 = ORIENTED_EDGE ( 'NONE', *, *, #14774, .T. ) ;
#12216 = DIRECTION ( 'NONE',  ( 1.000000000000000000, -0.000000000000000000, 0.000000000000000000 ) ) ;
#12217 = VECTOR ( 'NONE', #4619, 1000.000000000000000 ) ;
#12218 = VERTEX_POINT ( 'NONE', #14604 ) ;
#12219 = APPLICATION_PROTOCOL_DEFINITION ( 'draft international standard', 'automotive_design', 1998, #3906 ) ;
#12220 = EDGE_LOOP ( 'NONE', ( #1733, #16259 ) ) ;
#12221 = ORIENTED_EDGE ( 'NONE', *, *, #13038, .F. ) ;
#12222 = EDGE_CURVE ( 'NONE', #3705, #10179, #444, .T. ) ;
#12223 = DIRECTION ( 'NONE',  ( 1.000000000000000000, 0.000000000000000000, 0.000000000000000000 ) ) ;
#12224 = DIRECTION ( 'NONE',  ( 0.000000000000000000, -0.09950371902100807464, 0.9950371902099883759 ) ) ;
#12225 = EDGE_LOOP ( 'NONE', ( #10568, #6547, #6108, #12516 ) ) ;
#12226 = VECTOR ( 'NONE', #5376, 1000.000000000000000 ) ;
#12227 = DIRECTION ( 'NONE',  ( -0.000000000000000000, 1.000000000000000000, -0.000000000000000000 ) ) ;
#12228 = LINE ( 'NONE', #9747, #6749 ) ;
#12229 = VERTEX_POINT ( 'NONE', #526 ) ;
#12230 = EDGE_CURVE ( 'NONE', #14286, #15101, #15192, .T. ) ;
#12231 = DIRECTION ( 'NONE',  ( 0.000000000000000000, 0.000000000000000000, 1.000000000000000000 ) ) ;
#12232 = PRODUCT_DEFINITION_SHAPE ( 'NONE', 'NONE',  #2213 ) ;
#12233 = ORIENTED_EDGE ( 'NONE', *, *, #1710, .T. ) ;
#12234 = DIRECTION ( 'NONE',  ( 0.000000000000000000, 0.000000000000000000, -1.000000000000000000 ) ) ;
#12235 = DIRECTION ( 'NONE',  ( -0.000000000000000000, 1.000000000000000000, -0.000000000000000000 ) ) ;
#12236 = ORIENTED_EDGE ( 'NONE', *, *, #14213, .F. ) ;
#12237 = ORIENTED_EDGE ( 'NONE', *, *, #11586, .F. ) ;
#12239 = PLANE ( 'NONE',  #2338 ) ;
#12238 = CIRCLE ( 'NONE', #448, 20.75209553982835331 ) ;
#12240 = CIRCLE ( 'NONE', #11128, 2.500000000000002220 ) ;
#12241 = ORIENTED_EDGE ( 'NONE', *, *, #12196, .T. ) ;
#12242 = VERTEX_POINT ( 'NONE', #6695 ) ;
#12243 = DIRECTION ( 'NONE',  ( 0.000000000000000000, 0.000000000000000000, -1.000000000000000000 ) ) ;
#12244 = EDGE_CURVE ( 'NONE', #13085, #15297, #14641, .T. ) ;
#12245 = CARTESIAN_POINT ( 'NONE',  ( 55.99999999999989342, 473.6663340069157471, -531.5012393965008641 ) ) ;
#12246 = CARTESIAN_POINT ( 'NONE',  ( 40.00000000000000000, 68.00000000000000000, -25.99999999999999645 ) ) ;
#12247 = CARTESIAN_POINT ( 'NONE',  ( -36.00000000000000711, 8.000000000000000000, -19.00000000000000000 ) ) ;
#12248 = DIRECTION ( 'NONE',  ( 1.000000000000000000, 0.000000000000000000, 0.000000000000000000 ) ) ;
#12249 = EDGE_CURVE ( 'NONE', #12044, #2958, #16228, .T. ) ;
#12250 = EDGE_CURVE ( 'NONE', #15054, #1899, #14520, .T. ) ;
#12251 = AXIS2_PLACEMENT_3D ( 'NONE', #14330, #81, #3855 ) ;
#12252 = EDGE_CURVE ( 'NONE', #1386, #3583, #2014, .T. ) ;
#12253 = CARTESIAN_POINT ( 'NONE',  ( -2.764312543576804337, 191.4687391198921205, 37.59778641568980362 ) ) ;
#12254 = CIRCLE ( 'NONE', #12513, 3.300000000000004263 ) ;
#12255 = EDGE_CURVE ( 'NONE', #7845, #3903, #4221, .T. ) ;
#12256 = CARTESIAN_POINT ( 'NONE',  ( 39.99999999999999289, 10.00000000000000000, -26.00000000000000000 ) ) ;
#12257 = CARTESIAN_POINT ( 'NONE',  ( 40.00000000000000711, 19.00000000000000000, -26.00000000000000355 ) ) ;
#12258 = LINE ( 'NONE', #492, #14893 ) ;
#12259 = CYLINDRICAL_SURFACE ( 'NONE', #15465, 13.69540538389601991 ) ;
#12260 = DIRECTION ( 'NONE',  ( -1.000000000000000000, 0.000000000000000000, 0.000000000000000000 ) ) ;
#12262 = EDGE_LOOP ( 'NONE', ( #9994, #12630, #10688, #7684 ) ) ;
#12261 = VERTEX_POINT ( 'NONE', #16066 ) ;
#12263 = CARTESIAN_POINT ( 'NONE',  ( 56.72999999999999687, 289.4632308570088526, 37.52989836422092651 ) ) ;
#12264 = AXIS2_PLACEMENT_3D ( 'NONE', #5273, #233, #4355 ) ;
#12265 = CARTESIAN_POINT ( 'NONE',  ( -2.764312543581565418, 287.4577225941199004, 37.59778641568930624 ) ) ;
#12266 = AXIS2_PLACEMENT_3D ( 'NONE', #11144, #12346, #4536 ) ;
#12267 = DIRECTION ( 'NONE',  ( 0.000000000000000000, 0.9950371902099891530, 0.09950371902099770793 ) ) ;
#12268 = LINE ( 'NONE', #5552, #12706 ) ;
#12269 = ORIENTED_EDGE ( 'NONE', *, *, #3842, .T. ) ;
#12270 = CARTESIAN_POINT ( 'NONE',  ( 31.00000000000001776, 0.000000000000000000, -25.99999999999999645 ) ) ;
#12271 = ORIENTED_EDGE ( 'NONE', *, *, #4446, .T. ) ;
#12272 = LINE ( 'NONE', #12431, #3849 ) ;
#12273 = EDGE_CURVE ( 'NONE', #1865, #9809, #1197, .T. ) ;
#12274 = CARTESIAN_POINT ( 'NONE',  ( 0.000000000000000000, 289.4632308570086821, 37.52989836422091230 ) ) ;
#12275 = DIRECTION ( 'NONE',  ( 1.000000000000000000, -0.000000000000000000, 0.000000000000000000 ) ) ;
#12276 = CIRCLE ( 'NONE', #8147, 25.00000000000002132 ) ;
#12277 = FACE_OUTER_BOUND ( 'NONE', #13591, .T. ) ;
#12278 = DIRECTION ( 'NONE',  ( 0.000000000000000000, 0.000000000000000000, 1.000000000000000000 ) ) ;
#12279 = ORIENTED_EDGE ( 'NONE', *, *, #7090, .F. ) ;
#12280 = CARTESIAN_POINT ( 'NONE',  ( -5.000000000000000000, 0.000000000000000000, 0.000000000000000000 ) ) ;
#12281 = CARTESIAN_POINT ( 'NONE',  ( 8.420862748423350279E-16, 6.000000000000000000, 12.50000000000000000 ) ) ;
#12282 = ADVANCED_FACE ( 'NONE', ( #353, #13495 ), #1720, .T. ) ;
#12283 = DIRECTION ( 'NONE',  ( 1.000000000000000000, -0.000000000000000000, -0.000000000000000000 ) ) ;
#12284 = VECTOR ( 'NONE', #13442, 1000.000000000000000 ) ;
#12285 = EDGE_LOOP ( 'NONE', ( #16942, #970, #358, #8237 ) ) ;
#12286 = CARTESIAN_POINT ( 'NONE',  ( 35.00000000000003553, 3.000000000000000000, -20.99999999999999645 ) ) ;
#12287 = FACE_OUTER_BOUND ( 'NONE', #15390, .T. ) ;
#12288 = EDGE_LOOP ( 'NONE', ( #7712, #6921, #13773, #13046 ) ) ;
#12289 = DIRECTION ( 'NONE',  ( 0.000000000000000000, 0.000000000000000000, 1.000000000000000000 ) ) ;
#12290 = LINE ( 'NONE', #16230, #6807 ) ;
#12291 = CARTESIAN_POINT ( 'NONE',  ( -1.865551803243643184E-15, 286.2094592450220034, 37.20452120302224586 ) ) ;
#12292 = EDGE_LOOP ( 'NONE', ( #10057, #8765, #4229, #5770, #16240 ) ) ;
#12293 = LINE ( 'NONE', #3104, #1487 ) ;
#12294 = ORIENTED_EDGE ( 'NONE', *, *, #13604, .T. ) ;
#12295 = VERTEX_POINT ( 'NONE', #6949 ) ;
#12296 = CIRCLE ( 'NONE', #16128, 4.695405383896011919 ) ;
#12297 = CARTESIAN_POINT ( 'NONE',  ( 0.000000000000000000, 435.2933666400819561, -550.3792044179907634 ) ) ;
#12298 = VECTOR ( 'NONE', #8118, 1000.000000000000000 ) ;
#12299 = VERTEX_POINT ( 'NONE', #2931 ) ;
#12300 = ORIENTED_EDGE ( 'NONE', *, *, #9630, .F. ) ;
#12301 = LINE ( 'NONE', #16333, #278 ) ;
#12302 = VERTEX_POINT ( 'NONE', #12208 ) ;
#12303 = DIRECTION ( 'NONE',  ( 0.000000000000000000, -0.000000000000000000, -1.000000000000000000 ) ) ;
#12304 = DIRECTION ( 'NONE',  ( 0.000000000000000000, 0.000000000000000000, -1.000000000000000000 ) ) ;
#12305 = EDGE_LOOP ( 'NONE', ( #6327, #6515, #5332, #16130 ) ) ;
#12306 = CARTESIAN_POINT ( 'NONE',  ( -46.99999999999988631, 549.5810598491746077, -513.4200196135282113 ) ) ;
#12307 = AXIS2_PLACEMENT_3D ( 'NONE', #11038, #16110, #9416 ) ;
#12308 = DIRECTION ( 'NONE',  ( 0.000000000000000000, 0.000000000000000000, -1.000000000000000000 ) ) ;
#12309 = ORIENTED_EDGE ( 'NONE', *, *, #12153, .F. ) ;
#12310 = CARTESIAN_POINT ( 'NONE',  ( -31.00000000000000000, 19.00000000000000000, -31.00000000000000000 ) ) ;
#12311 = ORIENTED_EDGE ( 'NONE', *, *, #7068, .T. ) ;
#12312 = LINE ( 'NONE', #4501, #11881 ) ;
#12313 = ORIENTED_EDGE ( 'NONE', *, *, #4757, .T. ) ;
#12314 = ADVANCED_FACE ( 'NONE', ( #13236 ), #271, .T. ) ;
#12315 = ORIENTED_EDGE ( 'NONE', *, *, #11938, .T. ) ;
#12316 = SHAPE_REPRESENTATION ( 'Servo-Bas', ( #1488 ), #16822 ) ;
#12317 = ORIENTED_EDGE ( 'NONE', *, *, #3760, .T. ) ;
#12318 = EDGE_CURVE ( 'NONE', #851, #13578, #13009, .T. ) ;
#12319 = ADVANCED_FACE ( 'NONE', ( #13332 ), #4217, .T. ) ;
#12320 = ORIENTED_EDGE ( 'NONE', *, *, #4491, .T. ) ;
#12321 = DIRECTION ( 'NONE',  ( -1.000000000000000000, -0.000000000000000000, -0.000000000000000000 ) ) ;
#12322 = DIRECTION ( 'NONE',  ( 0.000000000000000000, 0.000000000000000000, 1.000000000000000000 ) ) ;
#12323 = CARTESIAN_POINT ( 'NONE',  ( -26.00000000000002132, 8.000000000000000000, 40.00000000000000711 ) ) ;
#12324 = VECTOR ( 'NONE', #11453, 1000.000000000000000 ) ;
#12325 = FACE_OUTER_BOUND ( 'NONE', #10198, .T. ) ;
#12326 = CARTESIAN_POINT ( 'NONE',  ( 31.00000000000000000, 11.00000000000000000, -26.00000000000000355 ) ) ;
#12327 = CARTESIAN_POINT ( 'NONE',  ( -1.725642888248489104, 190.2785135797052760, 37.61614439054951475 ) ) ;
#12328 = CYLINDRICAL_SURFACE ( 'NONE', #13126, 3.299999999999997158 ) ;
#12329 = CARTESIAN_POINT ( 'NONE',  ( 10.00000000000000000, 376.0487089519832011, -80.00000000000332534 ) ) ;
#12330 = FACE_BOUND ( 'NONE', #5408, .T. ) ;
#12331 = EDGE_CURVE ( 'NONE', #12394, #12986, #10817, .T. ) ;
#12332 = CARTESIAN_POINT ( 'NONE',  ( -3.000000000000002220, 60.00000000000000711, 6.000000000000000000 ) ) ;
#12333 = CARTESIAN_POINT ( 'NONE',  ( -3.000000000000000000, -1.836909530733565148E-16, 3.000000000000000000 ) ) ;
#12335 = EDGE_LOOP ( 'NONE', ( #9822, #1015 ) ) ;
#12334 = ORIENTED_EDGE ( 'NONE', *, *, #4583, .T. ) ;
#12336 = CARTESIAN_POINT ( 'NONE',  ( 40.00000000000000711, 11.00000000000000000, 25.99999999999999645 ) ) ;
#12337 = AXIS2_PLACEMENT_3D ( 'NONE', #5851, #2150, #1982 ) ;
#12338 = ADVANCED_FACE ( 'NONE', ( #3439 ), #6683, .F. ) ;
#12339 = ADVANCED_FACE ( 'NONE', ( #15286 ), #7285, .F. ) ;
#12340 = CARTESIAN_POINT ( 'NONE',  ( -54.99999999999999289, 515.4878487013597805, -546.7230258972048205 ) ) ;
#12341 = EDGE_CURVE ( 'NONE', #16177, #12025, #8503, .T. ) ;
#12342 = DIRECTION ( 'NONE',  ( 0.000000000000000000, -1.000000000000000000, 0.000000000000000000 ) ) ;
#12343 = CARTESIAN_POINT ( 'NONE',  ( -2.216159785453297477E-13, 106.2500000000000142, 0.000000000000000000 ) ) ;
#12344 = ORIENTED_EDGE ( 'NONE', *, *, #13616, .T. ) ;
#12345 = AXIS2_PLACEMENT_3D ( 'NONE', #11739, #6391, #5118 ) ;
#12346 = DIRECTION ( 'NONE',  ( -1.000000000000000000, 0.000000000000000000, 0.000000000000000000 ) ) ;
#12347 = VERTEX_POINT ( 'NONE', #16321 ) ;
#12348 = DIRECTION ( 'NONE',  ( 1.000000000000000000, -0.000000000000000000, 0.000000000000000000 ) ) ;
#12349 = VECTOR ( 'NONE', #12775, 1000.000000000000227 ) ;
#12350 = CARTESIAN_POINT ( 'NONE',  ( -2.467345170749102312, 191.0231794615329193, 37.60878752180607165 ) ) ;
#12351 = CARTESIAN_POINT ( 'NONE',  ( -37.00000000000000711, 0.000000000000000000, 23.00000000000000000 ) ) ;
#12352 = VECTOR ( 'NONE', #10134, 1000.000000000000000 ) ;
#12353 = PRODUCT_DEFINITION_SHAPE ( 'NONE', 'NONE',  #16975 ) ;
#12354 = LINE ( 'NONE', #514, #969 ) ;
#12355 =( NAMED_UNIT ( * ) PLANE_ANGLE_UNIT ( ) SI_UNIT ( $, .RADIAN. ) );
#12356 = EDGE_LOOP ( 'NONE', ( #4699, #132 ) ) ;
#12357 = FACE_OUTER_BOUND ( 'NONE', #10051, .T. ) ;
#12358 = EDGE_CURVE ( 'NONE', #6332, #10509, #10048, .T. ) ;
#12359 = ADVANCED_FACE ( 'NONE', ( #7363 ), #3963, .T. ) ;
#12360 = AXIS2_PLACEMENT_3D ( 'NONE', #10567, #14348, #3870 ) ;
#12361 = CARTESIAN_POINT ( 'NONE',  ( -55.99999999999989342, 549.5810598491749488, -575.3306267969850296 ) ) ;
#12362 = AXIS2_PLACEMENT_3D ( 'NONE', #315, #4010, #1516 ) ;
#12363 = EDGE_CURVE ( 'NONE', #6935, #14554, #4802, .T. ) ;
#12364 = APPLICATION_CONTEXT ( 'automotive_design' ) ;
#12365 = CARTESIAN_POINT ( 'NONE',  ( 22.99999999999998224, 0.000000000000000000, -31.00000000000003197 ) ) ;
#12366 = ORIENTED_EDGE ( 'NONE', *, *, #11105, .F. ) ;
#12367 = CARTESIAN_POINT ( 'NONE',  ( 10.00000000000000000, 340.8211049126788907, -341.7267989266199493 ) ) ;
#12368 = CARTESIAN_POINT ( 'NONE',  ( 0.000000000000000000, 301.0487089519837127, -150.0000000000038369 ) ) ;
#12369 = ORIENTED_EDGE ( 'NONE', *, *, #4830, .T. ) ;
#12370 = CARTESIAN_POINT ( 'NONE',  ( 5.941205806953520074, 0.000000000000000000, -15.14120580695351670 ) ) ;
#12371 = DIRECTION ( 'NONE',  ( 1.000000000000000000, 0.000000000000000000, 0.000000000000000000 ) ) ;
#12372 = LINE ( 'NONE', #4629, #13344 ) ;
#12373 = ORIENTED_EDGE ( 'NONE', *, *, #15919, .T. ) ;
#12374 = VECTOR ( 'NONE', #8304, 1000.000000000000114 ) ;
#12375 = VERTEX_POINT ( 'NONE', #12370 ) ;
#12376 = EDGE_LOOP ( 'NONE', ( #12504, #5785, #3485, #10907 ) ) ;
#12377 = CARTESIAN_POINT ( 'NONE',  ( -37.00000000000000000, 68.00000000000000000, 23.00000000000000355 ) ) ;
#12378 = SHAPE_DEFINITION_REPRESENTATION ( #6993, #1329 ) ;
#12379 = ORIENTED_EDGE ( 'NONE', *, *, #5501, .F. ) ;
#12380 = FACE_OUTER_BOUND ( 'NONE', #15783, .T. ) ;
#12381 = AXIS2_PLACEMENT_3D ( 'NONE', #4743, #7478, #13863 ) ;
#12382 = ORIENTED_EDGE ( 'NONE', *, *, #10786, .F. ) ;
#12383 = CARTESIAN_POINT ( 'NONE',  ( -23.00000000000002132, 10.00000000000000000, 37.00000000000000711 ) ) ;
#12384 = DIRECTION ( 'NONE',  ( 0.000000000000000000, 1.000000000000000000, 0.000000000000000000 ) ) ;
#12385 = ORIENTED_EDGE ( 'NONE', *, *, #5442, .T. ) ;
#12386 = DIRECTION ( 'NONE',  ( 0.000000000000000000, -1.000000000000000000, 0.000000000000000000 ) ) ;
#12387 = VECTOR ( 'NONE', #4108, 1000.000000000000000 ) ;
#12388 = DIRECTION ( 'NONE',  ( -0.000000000000000000, -1.000000000000000000, 0.000000000000000000 ) ) ;
#12389 = VERTEX_POINT ( 'NONE', #11241 ) ;
#12390 = CARTESIAN_POINT ( 'NONE',  ( 26.00000000000000000, 19.00000000000000000, 31.00000000000003197 ) ) ;
#12391 = ORIENTED_EDGE ( 'NONE', *, *, #15506, .F. ) ;
#12392 = ORIENTED_EDGE ( 'NONE', *, *, #11141, .T. ) ;
#12393 = VECTOR ( 'NONE', #9741, 1000.000000000000000 ) ;
#12394 = VERTEX_POINT ( 'NONE', #699 ) ;
#12395 = VECTOR ( 'NONE', #6735, 1000.000000000000000 ) ;
#12396 = ADVANCED_FACE ( 'NONE', ( #1889 ), #9963, .F. ) ;
#12397 = TOROIDAL_SURFACE ( 'NONE', #16774, 14.27500000000000036, 0.6999999999999999556 ) ;
#12398 = VECTOR ( 'NONE', #13321, 1000.000000000000000 ) ;
#12399 = ORIENTED_EDGE ( 'NONE', *, *, #9317, .F. ) ;
#12400 = ORIENTED_EDGE ( 'NONE', *, *, #10430, .F. ) ;
#12401 = CARTESIAN_POINT ( 'NONE',  ( -1.983673311716146026, 38.74097077230339892, 9.291669371308643122 ) ) ;
#12402 = FACE_OUTER_BOUND ( 'NONE', #1647, .T. ) ;
#12403 = CARTESIAN_POINT ( 'NONE',  ( 0.000000000000000000, 380.0000000000000000, 0.000000000000000000 ) ) ;
#12404 = AXIS2_PLACEMENT_3D ( 'NONE', #13680, #1902, #12472 ) ;
#12405 = PRODUCT_RELATED_PRODUCT_CATEGORY ( 'part', '', ( #7008 ) ) ;
#12406 = DIRECTION ( 'NONE',  ( 1.000000000000000000, 0.000000000000000000, -0.000000000000000000 ) ) ;
#12407 = CARTESIAN_POINT ( 'NONE',  ( 30.99999999999997868, 0.000000000000000000, -30.99999999999999645 ) ) ;
#12408 = LINE ( 'NONE', #648, #10991 ) ;
#12409 = AXIS2_PLACEMENT_3D ( 'NONE', #1011, #5274, #3673 ) ;
#12410 = DIRECTION ( 'NONE',  ( 0.000000000000000000, -1.000000000000000000, 2.220446049250308742E-15 ) ) ;
#12411 = VERTEX_POINT ( 'NONE', #3267 ) ;
#12412 = CARTESIAN_POINT ( 'NONE',  ( 0.000000000000000000, 372.8685141053778693, -86.48019484660871115 ) ) ;
#12413 = CARTESIAN_POINT ( 'NONE',  ( -45.00000000000000000, 493.2350855268092573, -585.2659423243250103 ) ) ;
#12414 = EDGE_CURVE ( 'NONE', #10866, #10664, #16827, .T. ) ;
#12415 = FACE_OUTER_BOUND ( 'NONE', #6463, .T. ) ;
#12416 = CARTESIAN_POINT ( 'NONE',  ( 10.00000000000000000, 396.9484440344699010, -165.7668752622531088 ) ) ;
#12418 = ORIENTED_EDGE ( 'NONE', *, *, #1998, .T. ) ;
#12417 = ORIENTED_EDGE ( 'NONE', *, *, #501, .F. ) ;
#12419 = CIRCLE ( 'NONE', #4998, 13.29999999999999893 ) ;
#12420 = CARTESIAN_POINT ( 'NONE',  ( 2.257948793614858118, 39.01519438325225053, 9.228844315538687226 ) ) ;
#12421 = VECTOR ( 'NONE', #11536, 1000.000000000000000 ) ;
#12422 = AXIS2_PLACEMENT_3D ( 'NONE', #2721, #12862, #1181 ) ;
#12423 = CARTESIAN_POINT ( 'NONE',  ( 394.0000000000001137, 240.7889724647196488, -104.9456657433598110 ) ) ;
#12424 = CARTESIAN_POINT ( 'NONE',  ( 55.99999999999989342, 559.9933750504617365, -542.0276205133087615 ) ) ;
#12425 = ORIENTED_EDGE ( 'NONE', *, *, #2728, .F. ) ;
#12426 = EDGE_CURVE ( 'NONE', #12389, #3004, #10266, .T. ) ;
#12427 = LINE ( 'NONE', #669, #8871 ) ;
#12428 = AXIS2_PLACEMENT_3D ( 'NONE', #5772, #5509, #14720 ) ;
#12429 = CARTESIAN_POINT ( 'NONE',  ( 0.3521046271560109298, 192.8092832092085587, 37.32951256787957561 ) ) ;
#12430 = VERTEX_POINT ( 'NONE', #3520 ) ;
#12431 = CARTESIAN_POINT ( 'NONE',  ( -33.99999999999997158, 3.000000000000000000, -22.99999999999999645 ) ) ;
#12432 = CARTESIAN_POINT ( 'NONE',  ( 0.2077619023754708749, 189.4340160014244248, 37.56638074116201409 ) ) ;
#12433 = CYLINDRICAL_SURFACE ( 'NONE', #15686, 0.7366000000000039183 ) ;
#12434 = ADVANCED_FACE ( 'NONE', ( #2135 ), #1969, .T. ) ;
#12435 = AXIS2_PLACEMENT_3D ( 'NONE', #13627, #11902, #5449 ) ;
#12436 = VECTOR ( 'NONE', #7965, 1000.000000000000000 ) ;
#12437 = CARTESIAN_POINT ( 'NONE',  ( 0.000000000000000000, 0.000000000000000000, 109.9999999999999858 ) ) ;
#12438 = AXIS2_PLACEMENT_3D ( 'NONE', #7011, #10891, #4366 ) ;
#12439 = DIRECTION ( 'NONE',  ( 1.000000000000000000, 0.000000000000000000, 0.000000000000000000 ) ) ;
#12440 = ORIENTED_EDGE ( 'NONE', *, *, #716, .F. ) ;
#12441 = CARTESIAN_POINT ( 'NONE',  ( -2.220446049250313081E-13, 135.5000000000000000, 0.000000000000000000 ) ) ;
#12442 = CIRCLE ( 'NONE', #2568, 0.5249999999999994671 ) ;
#12443 = DIRECTION ( 'NONE',  ( 1.000000000000000000, 0.000000000000000000, 0.000000000000000000 ) ) ;
#12444 = DIRECTION ( 'NONE',  ( -1.000000000000000000, 0.000000000000000000, 0.000000000000000000 ) ) ;
#12445 = MECHANICAL_DESIGN_GEOMETRIC_PRESENTATION_REPRESENTATION (  '', ( #2571 ), #1750 ) ;
#12446 = ORIENTED_EDGE ( 'NONE', *, *, #1654, .T. ) ;
#12447 = EDGE_CURVE ( 'NONE', #2065, #11864, #15203, .T. ) ;
#12448 = AXIS2_PLACEMENT_3D ( 'NONE', #15490, #15571, #7831 ) ;
#12449 = DIRECTION ( 'NONE',  ( 0.000000000000000000, 0.000000000000000000, -1.000000000000000000 ) ) ;
#12450 = DIRECTION ( 'NONE',  ( -6.123031769111888756E-17, -1.000000000000000000, 0.000000000000000000 ) ) ;
#12451 = VERTEX_POINT ( 'NONE', #943 ) ;
#12452 = DIRECTION ( 'NONE',  ( 1.156482317317875472E-15, 0.000000000000000000, 1.000000000000000000 ) ) ;
#12453 = VECTOR ( 'NONE', #7730, 1000.000000000000000 ) ;
#12454 = ADVANCED_FACE ( 'NONE', ( #7112 ), #11416, .T. ) ;
#12455 = DIRECTION ( 'NONE',  ( 1.000000000000000000, -0.000000000000000000, 0.000000000000000000 ) ) ;
#12456 = CARTESIAN_POINT ( 'NONE',  ( 0.000000000000000000, 620.7506394335853201, 109.9999999999999858 ) ) ;
#12457 = ORIENTED_EDGE ( 'NONE', *, *, #14219, .F. ) ;
#12458 = AXIS2_PLACEMENT_3D ( 'NONE', #7695, #15364, #14249 ) ;
#12459 = EDGE_CURVE ( 'NONE', #9495, #1506, #3188, .T. ) ;
#12460 = EDGE_CURVE ( 'NONE', #10318, #13387, #15468, .T. ) ;
#12461 = EDGE_CURVE ( 'NONE', #6723, #12507, #11166, .T. ) ;
#12462 = ORIENTED_EDGE ( 'NONE', *, *, #11410, .F. ) ;
#12463 = EDGE_LOOP ( 'NONE', ( #14574, #7226, #13913, #6091 ) ) ;
#12464 = AXIS2_PLACEMENT_3D ( 'NONE', #6862, #9464, #6700 ) ;
#12465 = CARTESIAN_POINT ( 'NONE',  ( -3.270000000000000462, 258.8496290447203592, 286.9685381829918924 ) ) ;
#12466 = AXIS2_PLACEMENT_3D ( 'NONE', #872, #12632, #10396 ) ;
#12467 = APPLICATION_PROTOCOL_DEFINITION ( 'draft international standard', 'automotive_design', 1998, #7630 ) ;
#12468 =( LENGTH_UNIT ( ) NAMED_UNIT ( * ) SI_UNIT ( .MILLI., .METRE. ) );
#12469 = VECTOR ( 'NONE', #2067, 1000.000000000000000 ) ;
#12470 = DIRECTION ( 'NONE',  ( 0.000000000000000000, 0.000000000000000000, 1.000000000000000000 ) ) ;
#12471 = ORIENTED_EDGE ( 'NONE', *, *, #387, .T. ) ;
#12472 = DIRECTION ( 'NONE',  ( 0.000000000000000000, 0.000000000000000000, 1.000000000000000000 ) ) ;
#12473 = LINE ( 'NONE', #625, #10275 ) ;
#12474 = AXIS2_PLACEMENT_3D ( 'NONE', #5155, #3633, #14364 ) ;
#12475 = EDGE_LOOP ( 'NONE', ( #1385, #7977, #12118, #2944 ) ) ;
#12476 = CARTESIAN_POINT ( 'NONE',  ( -25.99999999999999645, 0.000000000000000000, -39.99999999999999289 ) ) ;
#12477 = AXIS2_PLACEMENT_3D ( 'NONE', #4214, #12111, #14437 ) ;
#12478 = DIRECTION ( 'NONE',  ( 0.000000000000000000, 0.000000000000000000, -1.000000000000000000 ) ) ;
#12479 = ORIENTED_EDGE ( 'NONE', *, *, #2548, .F. ) ;
#12480 = ADVANCED_FACE ( 'NONE', ( #2390 ), #10301, .T. ) ;
#12481 = DIRECTION ( 'NONE',  ( 1.000000000000000000, 0.000000000000000000, -7.709882115452498874E-16 ) ) ;
#12482 = ORIENTED_EDGE ( 'NONE', *, *, #1324, .T. ) ;
#12483 = VERTEX_POINT ( 'NONE', #3941 ) ;
#12484 = VERTEX_POINT ( 'NONE', #10211 ) ;
#12485 = VERTEX_POINT ( 'NONE', #15538 ) ;
#12486 = ORIENTED_EDGE ( 'NONE', *, *, #13504, .T. ) ;
#12487 = FACE_OUTER_BOUND ( 'NONE', #10662, .T. ) ;
#12488 = AXIS2_PLACEMENT_3D ( 'NONE', #6825, #7949, #9257 ) ;
#12489 = EDGE_CURVE ( 'NONE', #6264, #9122, #8893, .T. ) ;
#12490 = LINE ( 'NONE', #733, #48 ) ;
#12491 = LINE ( 'NONE', #2173, #3942 ) ;
#12492 = CARTESIAN_POINT ( 'NONE',  ( -55.99999999999989342, 473.6663340069158039, -561.9448123979092315 ) ) ;
#12493 = CARTESIAN_POINT ( 'NONE',  ( -440.0000000000000568, 620.7506394335853201, 109.9999999999999858 ) ) ;
#12494 = DIRECTION ( 'NONE',  ( 0.000000000000000000, 1.000000000000000000, 0.000000000000000000 ) ) ;
#12495 = DIRECTION ( 'NONE',  ( 1.631319816340925608E-17, 0.000000000000000000, -1.000000000000000000 ) ) ;
#12496 = CARTESIAN_POINT ( 'NONE',  ( 0.000000000000000000, 264.4632308570090231, 287.5298983642207986 ) ) ;
#12497 = ORIENTED_EDGE ( 'NONE', *, *, #11959, .T. ) ;
#12498 = DIRECTION ( 'NONE',  ( -4.956352788505164254E-16, 0.000000000000000000, -1.000000000000000000 ) ) ;
#12499 = DIRECTION ( 'NONE',  ( 0.000000000000000000, -0.6468954956981580739, 0.7625786632508375629 ) ) ;
#12500 = CIRCLE ( 'NONE', #4325, 8.000000000000000000 ) ;
#12501 = VECTOR ( 'NONE', #13531, 1000.000000000000000 ) ;
#12502 = CARTESIAN_POINT ( 'NONE',  ( 54.99999999999999289, 515.4878487013597805, -631.7230258972047068 ) ) ;
#12503 = CARTESIAN_POINT ( 'NONE',  ( 394.0000000000001137, 339.3157724647196005, -16.41886574335978821 ) ) ;
#12505 = ORIENTED_EDGE ( 'NONE', *, *, #15868, .T. ) ;
#12504 = ORIENTED_EDGE ( 'NONE', *, *, #6312, .F. ) ;
#12506 = FACE_OUTER_BOUND ( 'NONE', #16945, .T. ) ;
#12507 = VERTEX_POINT ( 'NONE', #6492 ) ;
#12508 =( NAMED_UNIT ( * ) PLANE_ANGLE_UNIT ( ) SI_UNIT ( $, .RADIAN. ) );
#12509 = CARTESIAN_POINT ( 'NONE',  ( 0.7365999999999783832, 260.4765148507123058, 287.1312267635910871 ) ) ;
#12510 = CARTESIAN_POINT ( 'NONE',  ( 56.72999999999999687, 289.4632308570087957, 37.52989836422092651 ) ) ;
#12511 = VECTOR ( 'NONE', #512, 1000.000000000000000 ) ;
#12512 = VERTEX_POINT ( 'NONE', #1189 ) ;
#12513 = AXIS2_PLACEMENT_3D ( 'NONE', #5993, #11079, #8501 ) ;
#12514 = LINE ( 'NONE', #15263, #11063 ) ;
#12515 = CARTESIAN_POINT ( 'NONE',  ( 31.81980515339464333, 0.000000000000000000, -31.81980515339463622 ) ) ;
#12516 = ORIENTED_EDGE ( 'NONE', *, *, #14126, .T. ) ;
#12517 = CARTESIAN_POINT ( 'NONE',  ( 34.00000000000002842, 0.000000000000000000, 26.00000000000000355 ) ) ;
#12518 = DIRECTION ( 'NONE',  ( -0.000000000000000000, -0.000000000000000000, 1.000000000000000000 ) ) ;
#12519 = DIRECTION ( 'NONE',  ( -0.000000000000000000, -1.000000000000000000, -0.000000000000000000 ) ) ;
#12520 = DIRECTION ( 'NONE',  ( 0.000000000000000000, 0.000000000000000000, -1.000000000000000000 ) ) ;
#12521 = DIRECTION ( 'NONE',  ( -1.000000000000000000, 0.000000000000000000, -1.156482317317870344E-15 ) ) ;
#12522 = ORIENTED_EDGE ( 'NONE', *, *, #15681, .F. ) ;
#12523 = VECTOR ( 'NONE', #11930, 1000.000000000000000 ) ;
#12524 = LINE ( 'NONE', #3339, #139 ) ;
#12525 = EDGE_CURVE ( 'NONE', #5778, #219, #9172, .T. ) ;
#12526 = CIRCLE ( 'NONE', #11991, 3.000000000000002665 ) ;
#12527 = FACE_OUTER_BOUND ( 'NONE', #13158, .T. ) ;
#12528 = ORIENTED_EDGE ( 'NONE', *, *, #2677, .T. ) ;
#12529 = FACE_OUTER_BOUND ( 'NONE', #13277, .T. ) ;
#12530 = EDGE_CURVE ( 'NONE', #9375, #386, #11357, .T. ) ;
#12531 = ORIENTED_EDGE ( 'NONE', *, *, #15293, .T. ) ;
#12532 = DIRECTION ( 'NONE',  ( 0.000000000000000000, 0.000000000000000000, 1.000000000000000000 ) ) ;
#12533 = VECTOR ( 'NONE', #8544, 1000.000000000000000 ) ;
#12534 = CARTESIAN_POINT ( 'NONE',  ( 46.99999999999988631, 549.5810598491746077, -504.4200196135282113 ) ) ;
#12535 = EDGE_LOOP ( 'NONE', ( #5666, #995 ) ) ;
#12536 = CIRCLE ( 'NONE', #1827, 9.000000000000007105 ) ;
#12537 = DIRECTION ( 'NONE',  ( -0.000000000000000000, -1.000000000000000000, 0.000000000000000000 ) ) ;
#12538 = DIRECTION ( 'NONE',  ( 0.000000000000000000, 1.000000000000000000, 0.000000000000000000 ) ) ;
#12539 = CARTESIAN_POINT ( 'NONE',  ( 394.0000000000001137, 240.7889724647196488, -10.68226574335980139 ) ) ;
#12540 = VERTEX_POINT ( 'NONE', #8839 ) ;
#12541 = CARTESIAN_POINT ( 'NONE',  ( 26.00000000000000355, 19.00000000000000000, -31.00000000000003908 ) ) ;
#12542 = EDGE_LOOP ( 'NONE', ( #15414, #4292, #15547, #9867, #4046 ) ) ;
#12543 = ORIENTED_EDGE ( 'NONE', *, *, #12273, .T. ) ;
#12544 = DIRECTION ( 'NONE',  ( -1.000000000000000000, 0.000000000000000000, -0.000000000000000000 ) ) ;
#12545 = EDGE_CURVE ( 'NONE', #1812, #10736, #5867, .T. ) ;
#12546 = ITEM_DEFINED_TRANSFORMATION ( 'NONE', 'NONE', #3700,  #1488 ) ;
#12547 = AXIS2_PLACEMENT_3D ( 'NONE', #862, #3040, #15295 ) ;
#12548 = EDGE_CURVE ( 'NONE', #14448, #1410, #11086, .T. ) ;
#12549 = CARTESIAN_POINT ( 'NONE',  ( -3.000000000000000000, 6.000000000000000000, 3.000000000000000000 ) ) ;
#12550 = ADVANCED_FACE ( 'NONE', ( #1101 ), #15696, .F. ) ;
#12551 = EDGE_CURVE ( 'NONE', #5265, #12214, #13287, .T. ) ;
#12552 = EDGE_LOOP ( 'NONE', ( #14519, #10741, #15581, #3741, #1999, #11380, #2853, #7095 ) ) ;
#12553 = ADVANCED_FACE ( 'NONE', ( #8930 ), #4881, .T. ) ;
#12554 = CARTESIAN_POINT ( 'NONE',  ( -31.00000000000002842, 0.000000000000000000, -25.99999999999999645 ) ) ;
#12555 = CARTESIAN_POINT ( 'NONE',  ( 0.000000000000000000, 185.0000000000000284, -206.3519347178565795 ) ) ;
#12556 = ORIENTED_EDGE ( 'NONE', *, *, #13490, .T. ) ;
#12557 = CARTESIAN_POINT ( 'NONE',  ( 17.99999999999998224, 10.00000000000000000, -35.99999999999999289 ) ) ;
#12558 = CARTESIAN_POINT ( 'NONE',  ( 35.99999999999999289, 8.000000000000000000, 18.99999999999999289 ) ) ;
#12559 = ORIENTED_EDGE ( 'NONE', *, *, #7612, .F. ) ;
#12560 = AXIS2_PLACEMENT_3D ( 'NONE', #2121, #681, #8492 ) ;
#12561 = CARTESIAN_POINT ( 'NONE',  ( 10.00000000000000000, 301.0487089519837127, -150.0000000000038369 ) ) ;
#12562 = ORIENTED_EDGE ( 'NONE', *, *, #10343, .F. ) ;
#12563 = ORIENTED_EDGE ( 'NONE', *, *, #2144, .F. ) ;
#12564 = EDGE_LOOP ( 'NONE', ( #5774, #5945, #12182, #12639 ) ) ;
#12565 =( NAMED_UNIT ( * ) SI_UNIT ( $, .STERADIAN. ) SOLID_ANGLE_UNIT ( ) );
#12566 = ORIENTED_EDGE ( 'NONE', *, *, #7181, .F. ) ;
#12567 = ADVANCED_FACE ( 'NONE', ( #2306 ), #3034, .T. ) ;
#12568 = EDGE_CURVE ( 'NONE', #11607, #14915, #2468, .T. ) ;
#12569 = ORIENTED_EDGE ( 'NONE', *, *, #8214, .T. ) ;
#12570 = DIRECTION ( 'NONE',  ( -1.000000000000000000, 0.000000000000000000, -0.000000000000000000 ) ) ;
#12571 = EDGE_CURVE ( 'NONE', #1899, #11437, #14418, .T. ) ;
#12572 = AXIS2_PLACEMENT_3D ( 'NONE', #1923, #5791, #13371 ) ;
#12573 = CARTESIAN_POINT ( 'NONE',  ( 31.00000000000003553, 19.00000000000000000, 25.99999999999999645 ) ) ;
#12574 = CARTESIAN_POINT ( 'NONE',  ( -25.99999999999999645, 68.00000000000000000, -31.00000000000003197 ) ) ;
#12575 = DIRECTION ( 'NONE',  ( 0.000000000000000000, 0.000000000000000000, -1.000000000000000000 ) ) ;
#12576 = CARTESIAN_POINT ( 'NONE',  ( -55.99999999999989342, 473.6663340069157471, -531.5012393965008641 ) ) ;
#12577 = FACE_OUTER_BOUND ( 'NONE', #1131, .T. ) ;
#12578 = DIRECTION ( 'NONE',  ( 0.000000000000000000, -1.000000000000000000, 0.000000000000000000 ) ) ;
#12579 = CARTESIAN_POINT ( 'NONE',  ( 40.00000000000000711, 19.00000000000000000, -26.00000000000000355 ) ) ;
#12580 = EDGE_LOOP ( 'NONE', ( #15835, #12985, #9831, #5437 ) ) ;
#12581 = DIRECTION ( 'NONE',  ( 0.9998870921963913805, 0.01502673813723916230, 0.000000000000000000 ) ) ;
#12582 = DIRECTION ( 'NONE',  ( 0.000000000000000000, 0.000000000000000000, -1.000000000000000000 ) ) ;
#12583 = VECTOR ( 'NONE', #13048, 1000.000000000000000 ) ;
#12584 = DIRECTION ( 'NONE',  ( 0.000000000000000000, 0.9950371902099882648, 0.09950371902100807464 ) ) ;
#12586 = ORIENTED_EDGE ( 'NONE', *, *, #11825, .F. ) ;
#12585 = ORIENTED_EDGE ( 'NONE', *, *, #14983, .F. ) ;
#12587 = CARTESIAN_POINT ( 'NONE',  ( -19.00000000000001776, 10.00000000000000000, 40.00000000000000711 ) ) ;
#12588 = CARTESIAN_POINT ( 'NONE',  ( 394.0000000000001137, 234.3157724647196289, -104.2090657433598011 ) ) ;
#12589 = CARTESIAN_POINT ( 'NONE',  ( 175.0000000000000568, 515.4878487013597805, -521.7230258972047068 ) ) ;
#12590 = VERTEX_POINT ( 'NONE', #12952 ) ;
#12591 = PRODUCT_DEFINITION_SHAPE ( 'NONE', 'NONE',  #4837 ) ;
#12592 = PRODUCT_DEFINITION_CONTEXT ( 'detailed design', #12364, 'design' ) ;
#12593 = CARTESIAN_POINT ( 'NONE',  ( 17.00000000000000355, 380.0000000000000000, -44.71049682360899169 ) ) ;
#12594 = DIRECTION ( 'NONE',  ( 0.000000000000000000, 1.000000000000000000, 0.000000000000000000 ) ) ;
#12595 = ORIENTED_EDGE ( 'NONE', *, *, #12028, .F. ) ;
#12596 = DIRECTION ( 'NONE',  ( 0.000000000000000000, 1.000000000000000000, 0.000000000000000000 ) ) ;
#12597 = CARTESIAN_POINT ( 'NONE',  ( 0.000000000000000000, 240.7889724647196488, -17.15546574335979813 ) ) ;
#12598 = DIRECTION ( 'NONE',  ( 0.000000000000000000, 0.000000000000000000, -1.000000000000000000 ) ) ;
#12599 = VECTOR ( 'NONE', #16312, 1000.000000000000000 ) ;
#12600 = EDGE_CURVE ( 'NONE', #5055, #2354, #9184, .T. ) ;
#12601 = DIRECTION ( 'NONE',  ( 0.000000000000000000, 0.000000000000000000, -1.000000000000000000 ) ) ;
#12602 = DIRECTION ( 'NONE',  ( -0.000000000000000000, -0.000000000000000000, 1.000000000000000000 ) ) ;
#12603 = EDGE_CURVE ( 'NONE', #8443, #11999, #16725, .T. ) ;
#12604 = ORIENTED_EDGE ( 'NONE', *, *, #13612, .T. ) ;
#12605 = DIRECTION ( 'NONE',  ( 0.000000000000000000, 0.000000000000000000, -1.000000000000000000 ) ) ;
#12606 = CARTESIAN_POINT ( 'NONE',  ( 0.000000000000000000, 3.000000000000000000, 0.000000000000000000 ) ) ;
#12607 = EDGE_LOOP ( 'NONE', ( #10720, #13505, #12843, #270 ) ) ;
#12608 = VECTOR ( 'NONE', #14234, 1000.000000000000000 ) ;
#12609 = ORIENTED_EDGE ( 'NONE', *, *, #2887, .T. ) ;
#12610 = CARTESIAN_POINT ( 'NONE',  ( -45.00000000000000000, 493.2350855268086320, -494.4847040861889127 ) ) ;
#12611 = ADVANCED_FACE ( 'NONE', ( #9089 ), #16807, .F. ) ;
#12612 = CARTESIAN_POINT ( 'NONE',  ( 55.99999999999989342, 559.9933750504617365, -533.0276205133087615 ) ) ;
#12613 = ORIENTED_EDGE ( 'NONE', *, *, #8300, .T. ) ;
#12614 = DIRECTION ( 'NONE',  ( -0.000000000000000000, -0.000000000000000000, 1.000000000000000000 ) ) ;
#12615 = LINE ( 'NONE', #11327, #8742 ) ;
#12616 = CARTESIAN_POINT ( 'NONE',  ( 54.99999999999999289, 645.2345343053615352, -411.3640676610528999 ) ) ;
#12617 = VERTEX_POINT ( 'NONE', #14327 ) ;
#12618 = ADVANCED_BREP_SHAPE_REPRESENTATION ( '', ( #3067, #1488 ), #14944 ) ;
#12619 = SURFACE_STYLE_USAGE ( .BOTH. , #13920 ) ;
#12620 = CYLINDRICAL_SURFACE ( 'NONE', #12547, 7.500000000000000000 ) ;
#12621 = DIRECTION ( 'NONE',  ( 0.000000000000000000, 0.000000000000000000, -1.000000000000000000 ) ) ;
#12622 = ORIENTED_EDGE ( 'NONE', *, *, #14240, .T. ) ;
#12623 = EDGE_LOOP ( 'NONE', ( #6133, #2244, #12884, #6524 ) ) ;
#12624 = ADVANCED_FACE ( 'NONE', ( #13394 ), #15865, .F. ) ;
#12625 = AXIS2_PLACEMENT_3D ( 'NONE', #4157, #10771, #6724 ) ;
#12626 = CARTESIAN_POINT ( 'NONE',  ( 32.99999999999998579, 10.00000000000000000, 25.99999999999999645 ) ) ;
#12627 = CIRCLE ( 'NONE', #11786, 13.69540538389601991 ) ;
#12628 = PRODUCT_CONTEXT ( 'NONE', #16736, 'mechanical' ) ;
#12629 = CARTESIAN_POINT ( 'NONE',  ( 46.99999999999988631, 523.2161522479888163, -489.1982331128240276 ) ) ;
#12630 = ORIENTED_EDGE ( 'NONE', *, *, #10060, .F. ) ;
#12631 = CARTESIAN_POINT ( 'NONE',  ( 0.000000000000000000, 226.8713558223388134, -346.2582248962859808 ) ) ;
#12632 = DIRECTION ( 'NONE',  ( 0.000000000000000000, 0.000000000000000000, -1.000000000000000000 ) ) ;
#12633 = AXIS2_PLACEMENT_3D ( 'NONE', #1691, #7010, #11052 ) ;
#12634 = EDGE_CURVE ( 'NONE', #15298, #5706, #12187, .T. ) ;
#12635 = ORIENTED_EDGE ( 'NONE', *, *, #6107, .F. ) ;
#12636 = FACE_OUTER_BOUND ( 'NONE', #2496, .T. ) ;
#12637 = EDGE_CURVE ( 'NONE', #4318, #4133, #14766, .T. ) ;
#12638 = CARTESIAN_POINT ( 'NONE',  ( 0.000000000000000000, 339.1725919290084335, -110.6822657433597925 ) ) ;
#12639 = ORIENTED_EDGE ( 'NONE', *, *, #8582, .T. ) ;
#12640 = CARTESIAN_POINT ( 'NONE',  ( 0.000000000000000000, 38.00000000000000711, -5.741599279633704455E-16 ) ) ;
#12641 = EDGE_CURVE ( 'NONE', #3874, #13380, #334, .T. ) ;
#12642 = ORIENTED_EDGE ( 'NONE', *, *, #5354, .F. ) ;
#12643 = ORIENTED_EDGE ( 'NONE', *, *, #13102, .F. ) ;
#12644 = EDGE_CURVE ( 'NONE', #4130, #12617, #12627, .T. ) ;
#12645 = ADVANCED_FACE ( 'NONE', ( #5652 ), #5299, .F. ) ;
#12646 = ORIENTED_EDGE ( 'NONE', *, *, #9612, .T. ) ;
#12647 = SHAPE_REPRESENTATION_RELATIONSHIP ( 'NONE' , 'NONE' ,  #11761, #15684 ) ;
#12648 = CIRCLE ( 'NONE', #12112, 9.000000000000007105 ) ;
#12649 = EDGE_LOOP ( 'NONE', ( #15333, #11926, #8790, #9731 ) ) ;
#12650 = ORIENTED_EDGE ( 'NONE', *, *, #16540, .F. ) ;
#12651 = FACE_BOUND ( 'NONE', #12812, .T. ) ;
#12652 = DIRECTION ( 'NONE',  ( 0.000000000000000000, 0.000000000000000000, -1.000000000000000000 ) ) ;
#12653 = CARTESIAN_POINT ( 'NONE',  ( 0.000000000000000000, 0.000000000000000000, 0.000000000000000000 ) ) ;
#12654 = EDGE_CURVE ( 'NONE', #10282, #15314, #12013, .T. ) ;
#12655 = CARTESIAN_POINT ( 'NONE',  ( -3.270000000000000462, 258.7934930265975026, 287.5298983642207986 ) ) ;
#12656 = DIRECTION ( 'NONE',  ( 0.000000000000000000, 7.137148015447440312E-15, -1.000000000000000000 ) ) ;
#12657 = DIRECTION ( 'NONE',  ( -0.000000000000000000, 1.000000000000000000, -0.000000000000000000 ) ) ;
#12658 = CARTESIAN_POINT ( 'NONE',  ( -2.220446049250313081E-13, 135.5000000000000000, 0.000000000000000000 ) ) ;
#12659 = FACE_BOUND ( 'NONE', #102, .T. ) ;
#12660 = EDGE_CURVE ( 'NONE', #10621, #2722, #8144, .T. ) ;
#12661 = ORIENTED_EDGE ( 'NONE', *, *, #6875, .T. ) ;
#12662 = LINE ( 'NONE', #11535, #12806 ) ;
#12663 = PLANE ( 'NONE',  #11050 ) ;
#12664 = EDGE_CURVE ( 'NONE', #14463, #750, #2464, .T. ) ;
#12665 = EDGE_CURVE ( 'NONE', #4486, #11329, #8781, .T. ) ;
#12666 = ADVANCED_FACE ( 'NONE', ( #7961 ), #6758, .T. ) ;
#12667 = CIRCLE ( 'NONE', #7993, 9.000000000000007105 ) ;
#12668 =( GEOMETRIC_REPRESENTATION_CONTEXT ( 3 ) GLOBAL_UNCERTAINTY_ASSIGNED_CONTEXT ( ( #13232 ) ) GLOBAL_UNIT_ASSIGNED_CONTEXT ( ( #11724, #10183, #16782 ) ) REPRESENTATION_CONTEXT ( 'NONE', 'WORKASPACE' ) );
#12669 = PLANE ( 'NONE',  #5189 ) ;
#12671 = ORIENTED_EDGE ( 'NONE', *, *, #7724, .T. ) ;
#12670 = ORIENTED_EDGE ( 'NONE', *, *, #7184, .F. ) ;
#12672 = DIRECTION ( 'NONE',  ( -0.000000000000000000, -1.000000000000000000, -0.000000000000000000 ) ) ;
#12673 = ORIENTED_EDGE ( 'NONE', *, *, #11590, .F. ) ;
#12674 = VECTOR ( 'NONE', #10994, 1000.000000000000000 ) ;
#12675 = DIRECTION ( 'NONE',  ( 0.000000000000000000, 1.000000000000000000, 1.224646799147353207E-16 ) ) ;
#12676 = DIRECTION ( 'NONE',  ( -1.000000000000000000, -0.000000000000000000, -0.000000000000000000 ) ) ;
#12677 = VECTOR ( 'NONE', #5656, 1000.000000000000000 ) ;
#12678 = EDGE_LOOP ( 'NONE', ( #15334, #1445, #4674, #14294 ) ) ;
#12679 = VECTOR ( 'NONE', #16791, 1000.000000000000000 ) ;
#12680 = VECTOR ( 'NONE', #12069, 1000.000000000000000 ) ;
#12681 = LINE ( 'NONE', #8738, #16273 ) ;
#12682 = DIRECTION ( 'NONE',  ( 1.000000000000000000, 0.000000000000000000, 0.000000000000000000 ) ) ;
#12683 = ORIENTED_EDGE ( 'NONE', *, *, #7487, .F. ) ;
#12684 = CARTESIAN_POINT ( 'NONE',  ( -23.00000000000002132, 10.00000000000000000, 37.00000000000000711 ) ) ;
#12685 = DIRECTION ( 'NONE',  ( -1.000000000000000000, -0.000000000000000000, -0.000000000000000000 ) ) ;
#12686 = CARTESIAN_POINT ( 'NONE',  ( -55.99999999999989342, 493.2350855268086320, -521.8755148539809170 ) ) ;
#12687 = AXIS2_PLACEMENT_3D ( 'NONE', #11413, #13044, #16646 ) ;
#12688 = ADVANCED_FACE ( 'NONE', ( #10549 ), #8223, .F. ) ;
#12689 = CARTESIAN_POINT ( 'NONE',  ( -46.99999999999988631, 559.9933750504617365, -542.0276205133087615 ) ) ;
#12690 = DIRECTION ( 'NONE',  ( -1.000000000000000000, -0.000000000000000000, 3.854941057726247958E-16 ) ) ;
#12691 = VERTEX_POINT ( 'NONE', #9437 ) ;
#12692 = CARTESIAN_POINT ( 'NONE',  ( 75.00000000000000000, 380.0000000000000000, 0.000000000000000000 ) ) ;
#12693 = AXIS2_PLACEMENT_3D ( 'NONE', #16028, #10618, #1518 ) ;
#12694 = CIRCLE ( 'NONE', #14334, 22.50000000000000000 ) ;
#12695 = DIRECTION ( 'NONE',  ( 0.000000000000000000, 1.000000000000000000, 0.000000000000000000 ) ) ;
#12696 = CARTESIAN_POINT ( 'NONE',  ( -26.00000000000000000, 11.00000000000000000, -31.00000000000003908 ) ) ;
#12697 = AXIS2_PLACEMENT_3D ( 'NONE', #15443, #16721, #5042 ) ;
#12698 = VERTEX_POINT ( 'NONE', #14846 ) ;
#12699 = CARTESIAN_POINT ( 'NONE',  ( 29.68009836720079875, 352.3758082234937206, 0.000000000000000000 ) ) ;
#12700 = EDGE_CURVE ( 'NONE', #9884, #12375, #15636, .T. ) ;
#12701 = VECTOR ( 'NONE', #1237, 1000.000000000000000 ) ;
#12702 = DIRECTION ( 'NONE',  ( 1.000000000000000000, -0.000000000000000000, 0.000000000000000000 ) ) ;
#12703 = VERTEX_POINT ( 'NONE', #15784 ) ;
#12704 = CARTESIAN_POINT ( 'NONE',  ( -3.270000000000000462, 30.59170509404782479, 305.9170509405147982 ) ) ;
#12705 = AXIS2_PLACEMENT_3D ( 'NONE', #6540, #16688, #10265 ) ;
#12706 = VECTOR ( 'NONE', #9523, 1000.000000000000000 ) ;
#12707 = FACE_BOUND ( 'NONE', #7249, .T. ) ;
#12708 = DIRECTION ( 'NONE',  ( -1.000000000000000000, -0.000000000000000000, -0.000000000000000000 ) ) ;
#12709 = ORIENTED_EDGE ( 'NONE', *, *, #8324, .F. ) ;
#12710 = EDGE_CURVE ( 'NONE', #11402, #10409, #4029, .T. ) ;
#12711 = CARTESIAN_POINT ( 'NONE',  ( -55.99999999999989342, 523.2161522479888163, -489.1982331128240276 ) ) ;
#12712 = PRESENTATION_STYLE_ASSIGNMENT (( #14083 ) ) ;
#12713 = CARTESIAN_POINT ( 'NONE',  ( -3.165718926339639694, 286.4868066975118381, 37.56780454546780845 ) ) ;
#12714 = ORIENTED_EDGE ( 'NONE', *, *, #4876, .T. ) ;
#12715 = AXIS2_PLACEMENT_3D ( 'NONE', #7052, #14804, #14883 ) ;
#12716 = CARTESIAN_POINT ( 'NONE',  ( 30.99999999999999645, 68.00000000000000000, 31.00000000000001066 ) ) ;
#12717 = ITEM_DEFINED_TRANSFORMATION ( 'NONE', 'NONE', #16834,  #1488 ) ;
#12718 =( GEOMETRIC_REPRESENTATION_CONTEXT ( 3 ) GLOBAL_UNCERTAINTY_ASSIGNED_CONTEXT ( ( #4307 ) ) GLOBAL_UNIT_ASSIGNED_CONTEXT ( ( #12057, #16169, #16087 ) ) REPRESENTATION_CONTEXT ( 'NONE', 'WORKASPACE' ) );
#12719 = CIRCLE ( 'NONE', #14919, 14.27500000000000036 ) ;
#12720 = PRODUCT_DEFINITION ( 'UNKNOWN', '', #5885, #11222 ) ;
#12721 =( NAMED_UNIT ( * ) PLANE_ANGLE_UNIT ( ) SI_UNIT ( $, .RADIAN. ) );
#12722 = VECTOR ( 'NONE', #7650, 1000.000000000000000 ) ;
#12723 = CARTESIAN_POINT ( 'NONE',  ( 10.00000000000000000, 309.2289037985885898, -79.88019484660914316 ) ) ;
#12724 = EDGE_LOOP ( 'NONE', ( #13119, #3615, #8507, #15566 ) ) ;
#12725 = AXIS2_PLACEMENT_3D ( 'NONE', #7769, #15675, #4013 ) ;
#12726 = DIRECTION ( 'NONE',  ( 0.000000000000000000, -1.000000000000000000, 0.000000000000000000 ) ) ;
#12727 = DIRECTION ( 'NONE',  ( -0.000000000000000000, 1.000000000000000000, -0.000000000000000000 ) ) ;
#12728 = VECTOR ( 'NONE', #11435, 1000.000000000000000 ) ;
#12729 = ORIENTED_EDGE ( 'NONE', *, *, #1526, .T. ) ;
#12730 = DIRECTION ( 'NONE',  ( -1.000000000000000000, 0.000000000000000000, 0.000000000000000000 ) ) ;
#12731 = CARTESIAN_POINT ( 'NONE',  ( 22.99999999999995737, 3.000000000000000000, -36.99999999999999289 ) ) ;
#12732 = ORIENTED_EDGE ( 'NONE', *, *, #7286, .F. ) ;
#12733 = CIRCLE ( 'NONE', #14929, 4.000164074322309027 ) ;
#12734 = CARTESIAN_POINT ( 'NONE',  ( -55.99999999999989342, 549.5810598491746077, -504.4200196135282113 ) ) ;
#12735 = VECTOR ( 'NONE', #10753, 1000.000000000000000 ) ;
#12736 = VERTEX_POINT ( 'NONE', #2909 ) ;
#12737 = ORIENTED_EDGE ( 'NONE', *, *, #10522, .T. ) ;
#12738 = CIRCLE ( 'NONE', #2595, 18.50000000000000000 ) ;
#12739 = ORIENTED_EDGE ( 'NONE', *, *, #5524, .F. ) ;
#12740 = EDGE_CURVE ( 'NONE', #11672, #7276, #14505, .T. ) ;
#12741 = ORIENTED_EDGE ( 'NONE', *, *, #13635, .T. ) ;
#12742 = ORIENTED_EDGE ( 'NONE', *, *, #2291, .T. ) ;
#12743 = CIRCLE ( 'NONE', #10545, 14.59999999999999964 ) ;
#12744 = DIRECTION ( 'NONE',  ( -0.000000000000000000, -1.000000000000000000, -0.000000000000000000 ) ) ;
#12745 = DIRECTION ( 'NONE',  ( -0.000000000000000000, -0.000000000000000000, 1.000000000000000000 ) ) ;
#12746 = EDGE_CURVE ( 'NONE', #7389, #2600, #6563, .T. ) ;
#12747 = CARTESIAN_POINT ( 'NONE',  ( -2.220446049250313081E-13, 135.5000000000000000, 0.000000000000000000 ) ) ;
#12748 = CARTESIAN_POINT ( 'NONE',  ( -20.00000000000003197, 3.000000000000000000, 40.00000000000000711 ) ) ;
#12749 = LINE ( 'NONE', #3645, #2300 ) ;
#12750 = CARTESIAN_POINT ( 'NONE',  ( -31.00000000000000000, 8.000000000000000000, -31.00000000000000000 ) ) ;
#12751 = CARTESIAN_POINT ( 'NONE',  ( 54.99999999999999289, 515.4878487013597805, -546.7230258972048205 ) ) ;
#12752 = ORIENTED_EDGE ( 'NONE', *, *, #11387, .F. ) ;
#12753 = DIRECTION ( 'NONE',  ( -0.000000000000000000, -0.000000000000000000, -1.000000000000000000 ) ) ;
#12754 = LINE ( 'NONE', #15653, #11325 ) ;
#12755 = ORIENTED_EDGE ( 'NONE', *, *, #8365, .T. ) ;
#12756 = LINE ( 'NONE', #6457, #4409 ) ;
#12758 = ORIENTED_EDGE ( 'NONE', *, *, #6231, .T. ) ;
#12757 = ORIENTED_EDGE ( 'NONE', *, *, #15068, .T. ) ;
#12759 = LINE ( 'NONE', #7587, #15521 ) ;
#12760 = EDGE_CURVE ( 'NONE', #5894, #13073, #4401, .T. ) ;
#12761 = AXIS2_PLACEMENT_3D ( 'NONE', #5570, #7884, #13137 ) ;
#12762 = ORIENTED_EDGE ( 'NONE', *, *, #2268, .T. ) ;
#12763 = DIRECTION ( 'NONE',  ( 0.000000000000000000, 0.000000000000000000, 1.000000000000000000 ) ) ;
#12764 = LINE ( 'NONE', #11388, #3861 ) ;
#12765 = EDGE_CURVE ( 'NONE', #12691, #16882, #16461, .T. ) ;
#12766 = LINE ( 'NONE', #5180, #9139 ) ;
#12767 = ADVANCED_FACE ( 'NONE', ( #3417 ), #13649, .F. ) ;
#12769 = ORIENTED_EDGE ( 'NONE', *, *, #8682, .T. ) ;
#12768 = EDGE_CURVE ( 'NONE', #7178, #5457, #15001, .T. ) ;
#12770 = ADVANCED_FACE ( 'NONE', ( #11306 ), #1657, .F. ) ;
#12771 = UNCERTAINTY_MEASURE_WITH_UNIT (LENGTH_MEASURE( 1.000000000000000082E-05 ), #4230, 'distance_accuracy_value', 'NONE');
#12772 = DIRECTION ( 'NONE',  ( -0.000000000000000000, -1.000000000000000000, -0.000000000000000000 ) ) ;
#12773 = CARTESIAN_POINT ( 'NONE',  ( -26.00000000000000000, 19.00000000000000000, -31.00000000000003908 ) ) ;
#12774 = ORIENTED_EDGE ( 'NONE', *, *, #3295, .T. ) ;
#12775 = DIRECTION ( 'NONE',  ( 3.491481338843132566E-15, 0.9950371902099890420, -0.09950371902099952592 ) ) ;
#12776 = VECTOR ( 'NONE', #2207, 1000.000000000000000 ) ;
#12777 = CARTESIAN_POINT ( 'NONE',  ( 0.1218274893879093684, 193.1239507390138215, 37.43226525377765768 ) ) ;
#12778 = FACE_OUTER_BOUND ( 'NONE', #7027, .T. ) ;
#12779 = FACE_OUTER_BOUND ( 'NONE', #12580, .T. ) ;
#12780 = DIRECTION ( 'NONE',  ( 1.104713198929451483E-16, 0.09950371902099953980, 0.9950371902099890420 ) ) ;
#12781 = ORIENTED_EDGE ( 'NONE', *, *, #4791, .T. ) ;
#12782 = LINE ( 'NONE', #11482, #14973 ) ;
#12783 = VECTOR ( 'NONE', #1359, 1000.000000000000000 ) ;
#12784 = CARTESIAN_POINT ( 'NONE',  ( -55.99999999999989342, 473.6663340069157471, -531.5012393965008641 ) ) ;
#12785 = AXIS2_PLACEMENT_3D ( 'NONE', #13101, #10512, #11892 ) ;
#12786 = LINE ( 'NONE', #8671, #5268 ) ;
#12787 = EDGE_LOOP ( 'NONE', ( #10105, #16395, #3548, #7016 ) ) ;
#12788 = ADVANCED_FACE ( 'NONE', ( #4613 ), #4779, .T. ) ;
#12789 = FACE_OUTER_BOUND ( 'NONE', #7045, .T. ) ;
#12790 = CARTESIAN_POINT ( 'NONE',  ( -45.00000000000000000, 473.6663340069158039, -561.9448123979092315 ) ) ;
#12791 = ORIENTED_EDGE ( 'NONE', *, *, #6753, .T. ) ;
#12792 = CARTESIAN_POINT ( 'NONE',  ( -55.99999999999989342, 549.5810598491746077, -518.1154249974242703 ) ) ;
#12793 = LINE ( 'NONE', #10302, #15860 ) ;
#12794 = DIRECTION ( 'NONE',  ( 0.000000000000000000, 0.000000000000000000, 1.000000000000000000 ) ) ;
#12795 = ORIENTED_EDGE ( 'NONE', *, *, #5181, .T. ) ;
#12796 = AXIS2_PLACEMENT_3D ( 'NONE', #11061, #3333, #11147 ) ;
#12797 = VECTOR ( 'NONE', #8141, 1000.000000000000000 ) ;
#12798 = SURFACE_STYLE_USAGE ( .BOTH. , #11755 ) ;
#12799 = FACE_OUTER_BOUND ( 'NONE', #16247, .T. ) ;
#12800 = CARTESIAN_POINT ( 'NONE',  ( 5.044974746830580337, 0.000000000000000000, 0.000000000000000000 ) ) ;
#12801 = ORIENTED_EDGE ( 'NONE', *, *, #4465, .F. ) ;
#12802 = EDGE_CURVE ( 'NONE', #3021, #7963, #12272, .T. ) ;
#12803 = DIRECTION ( 'NONE',  ( -0.000000000000000000, -1.000000000000000000, -0.000000000000000000 ) ) ;
#12804 = ADVANCED_FACE ( 'NONE', ( #16547 ), #15180, .T. ) ;
#12805 = CONTEXT_DEPENDENT_SHAPE_REPRESENTATION ( #7528, #5626 ) ;
#12806 = VECTOR ( 'NONE', #11712, 1000.000000000000000 ) ;
#12807 = ORIENTED_EDGE ( 'NONE', *, *, #10246, .T. ) ;
#12808 = AXIS2_PLACEMENT_3D ( 'NONE', #2284, #14465, #3990 ) ;
#12809 = FACE_OUTER_BOUND ( 'NONE', #6618, .T. ) ;
#12810 = CARTESIAN_POINT ( 'NONE',  ( 22.99999999999995737, 3.000000000000000000, -36.99999999999999289 ) ) ;
#12811 = CARTESIAN_POINT ( 'NONE',  ( 31.00000000000000000, 11.00000000000000000, 30.99999999999999289 ) ) ;
#12812 = EDGE_LOOP ( 'NONE', ( #6983, #14637 ) ) ;
#12813 = CARTESIAN_POINT ( 'NONE',  ( 37.00000000000003553, 3.000000000000000000, 20.00000000000000000 ) ) ;
#12814 = LINE ( 'NONE', #16669, #2903 ) ;
#12815 = ORIENTED_EDGE ( 'NONE', *, *, #3072, .F. ) ;
#12816 = DIRECTION ( 'NONE',  ( 0.000000000000000000, -0.9950371902099900412, 0.09950371902098976984 ) ) ;
#12817 = ORIENTED_EDGE ( 'NONE', *, *, #11735, .T. ) ;
#12818 = VERTEX_POINT ( 'NONE', #8572 ) ;
#12819 = FACE_OUTER_BOUND ( 'NONE', #9470, .T. ) ;
#12820 = VERTEX_POINT ( 'NONE', #8486 ) ;
#12821 = CARTESIAN_POINT ( 'NONE',  ( 39.41161623800085323, 323.9612906317821057, 0.000000000000000000 ) ) ;
#12822 = VERTEX_POINT ( 'NONE', #12517 ) ;
#12823 = ORIENTED_EDGE ( 'NONE', *, *, #3109, .F. ) ;
#12824 = DIRECTION ( 'NONE',  ( 0.000000000000000000, 1.000000000000000000, 0.000000000000000000 ) ) ;
#12825 = DIRECTION ( 'NONE',  ( 1.000000000000000000, 0.000000000000000000, 0.000000000000000000 ) ) ;
#12826 = VECTOR ( 'NONE', #12780, 1000.000000000000227 ) ;
#12827 = DIRECTION ( 'NONE',  ( -1.000000000000000000, 0.000000000000000000, -0.000000000000000000 ) ) ;
#12828 = CARTESIAN_POINT ( 'NONE',  ( -40.00000000000000000, 68.00000000000000000, 26.00000000000000355 ) ) ;
#12829 = DIRECTION ( 'NONE',  ( 6.123031769111888756E-17, 0.000000000000000000, 1.000000000000000000 ) ) ;
#12830 = EDGE_CURVE ( 'NONE', #3860, #6348, #1369, .T. ) ;
#12831 = CARTESIAN_POINT ( 'NONE',  ( 31.00000000000004263, 68.00000000000000000, -25.99999999999999645 ) ) ;
#12832 = DIRECTION ( 'NONE',  ( 0.6294249519366466039, -0.7770612780724246438, 9.516256069327462658E-17 ) ) ;
#12833 = ORIENTED_EDGE ( 'NONE', *, *, #6661, .T. ) ;
#12834 = LINE ( 'NONE', #3812, #484 ) ;
#12835 = FACE_BOUND ( 'NONE', #15509, .T. ) ;
#12836 = ORIENTED_EDGE ( 'NONE', *, *, #13422, .F. ) ;
#12837 = PLANE ( 'NONE',  #6861 ) ;
#12839 = EDGE_LOOP ( 'NONE', ( #13640, #12233 ) ) ;
#12838 = ORIENTED_EDGE ( 'NONE', *, *, #16434, .F. ) ;
#12840 = EDGE_CURVE ( 'NONE', #5865, #12261, #10975, .T. ) ;
#12841 = DIRECTION ( 'NONE',  ( -0.000000000000000000, 1.000000000000000000, -0.000000000000000000 ) ) ;
#12842 = AXIS2_PLACEMENT_3D ( 'NONE', #486, #8460, #5877 ) ;
#12843 = ORIENTED_EDGE ( 'NONE', *, *, #13269, .T. ) ;
#12844 = CARTESIAN_POINT ( 'NONE',  ( -3.270000000000002238, 239.4632308570078294, 86.73739990498292229 ) ) ;
#12845 = DIRECTION ( 'NONE',  ( -0.000000000000000000, -1.000000000000000000, -0.000000000000000000 ) ) ;
#12846 = ORIENTED_EDGE ( 'NONE', *, *, #15354, .T. ) ;
#12847 = DIRECTION ( 'NONE',  ( 1.000000000000000000, 0.000000000000000000, 0.000000000000000000 ) ) ;
#12849 = EDGE_CURVE ( 'NONE', #13944, #10509, #16180, .T. ) ;
#12848 = ORIENTED_EDGE ( 'NONE', *, *, #3841, .T. ) ;
#12850 = DIRECTION ( 'NONE',  ( -1.000000000000000000, 0.000000000000000000, 0.000000000000000000 ) ) ;
#12851 = AXIS2_PLACEMENT_3D ( 'NONE', #8504, #12455, #9879 ) ;
#12852 = CARTESIAN_POINT ( 'NONE',  ( 31.81980515339464333, 0.000000000000000000, -35.11980515339463693 ) ) ;
#12853 = CARTESIAN_POINT ( 'NONE',  ( 26.00000000000000355, 11.00000000000000000, -31.00000000000004263 ) ) ;
#12854 = DIRECTION ( 'NONE',  ( 0.000000000000000000, -0.8660254037844363761, -0.5000000000000039968 ) ) ;
#12855 = DIRECTION ( 'NONE',  ( 0.000000000000000000, 0.000000000000000000, 1.000000000000000000 ) ) ;
#12856 = VERTEX_POINT ( 'NONE', #3172 ) ;
#12857 = ADVANCED_FACE ( 'NONE', ( #8408 ), #13463, .T. ) ;
#12858 = ADVANCED_FACE ( 'NONE', ( #4688 ), #16302, .F. ) ;
#12859 = CARTESIAN_POINT ( 'NONE',  ( -26.00000000000000000, 19.00000000000000000, -40.00000000000000711 ) ) ;
#12860 = EDGE_CURVE ( 'NONE', #985, #8625, #9785, .T. ) ;
#12861 = DIRECTION ( 'NONE',  ( 1.000000000000000000, -0.000000000000000000, -0.000000000000000000 ) ) ;
#12862 = DIRECTION ( 'NONE',  ( -0.000000000000000000, -1.000000000000000000, 0.000000000000000000 ) ) ;
#12863 = VERTEX_POINT ( 'NONE', #7765 ) ;
#12864 = CARTESIAN_POINT ( 'NONE',  ( -21.00000000000002842, 3.000000000000000000, -32.49999999999999289 ) ) ;
#12865 = AXIS2_PLACEMENT_3D ( 'NONE', #2178, #14035, #14129 ) ;
#12866 = CARTESIAN_POINT ( 'NONE',  ( -55.99999999999988631, 172.2913238082672933, 146.1547335252150788 ) ) ;
#12867 = EDGE_LOOP ( 'NONE', ( #15976, #7846 ) ) ;
#12868 = CARTESIAN_POINT ( 'NONE',  ( 449.9999999999998295, 135.5000000000000000, 3.000000000000000000 ) ) ;
#12869 = CARTESIAN_POINT ( 'NONE',  ( -39.99999999999997868, 3.000000000000000000, 26.00000000000000355 ) ) ;
#12870 = FACE_OUTER_BOUND ( 'NONE', #5356, .T. ) ;
#12871 = ORIENTED_EDGE ( 'NONE', *, *, #15591, .T. ) ;
#12872 = PRODUCT_DEFINITION_SHAPE ( 'NONE', 'NONE',  #12720 ) ;
#12873 = DIRECTION ( 'NONE',  ( 0.000000000000000000, -0.09950371902100807464, 0.9950371902099883759 ) ) ;
#12874 = DIRECTION ( 'NONE',  ( 0.000000000000000000, -0.7711125544961918710, -0.6366988521258363232 ) ) ;
#12875 = LINE ( 'NONE', #6326, #1707 ) ;
#12876 = ORIENTED_EDGE ( 'NONE', *, *, #2254, .T. ) ;
#12877 = EDGE_CURVE ( 'NONE', #10758, #5421, #10286, .T. ) ;
#12878 = EDGE_CURVE ( 'NONE', #10947, #13251, #2446, .T. ) ;
#12879 = CARTESIAN_POINT ( 'NONE',  ( 10.00000000000000000, 301.0487089519826327, 2.148629195649657075E-12 ) ) ;
#12880 = EDGE_CURVE ( 'NONE', #3047, #10332, #14058, .T. ) ;
#12881 = ITEM_DEFINED_TRANSFORMATION ( 'NONE', 'NONE', #408,  #1488 ) ;
#12882 = AXIS2_PLACEMENT_3D ( 'NONE', #4485, #8515, #9736 ) ;
#12883 = CARTESIAN_POINT ( 'NONE',  ( 0.000000000000000000, 0.000000000000000000, 0.000000000000000000 ) ) ;
#12884 = ORIENTED_EDGE ( 'NONE', *, *, #10430, .T. ) ;
#12885 = DIRECTION ( 'NONE',  ( 0.000000000000000000, 0.000000000000000000, -1.000000000000000000 ) ) ;
#12886 = CARTESIAN_POINT ( 'NONE',  ( 17.99999999999998579, 6.000000000000000000, -36.99999999999999289 ) ) ;
#12887 = DIRECTION ( 'NONE',  ( 1.000000000000000000, -0.000000000000000000, 0.000000000000000000 ) ) ;
#12888 = ORIENTED_EDGE ( 'NONE', *, *, #7393, .F. ) ;
#12889 = CARTESIAN_POINT ( 'NONE',  ( 10.00000000000000000, 306.0487089519832011, -75.00000000000380851 ) ) ;
#12890 = DIRECTION ( 'NONE',  ( -0.000000000000000000, -1.000000000000000000, -0.000000000000000000 ) ) ;
#12891 = EDGE_LOOP ( 'NONE', ( #668, #1888, #9240, #7446 ) ) ;
#12892 = VECTOR ( 'NONE', #3314, 1000.000000000000114 ) ;
#12893 = AXIS2_PLACEMENT_3D ( 'NONE', #13806, #4538, #13892 ) ;
#12894 = FACE_OUTER_BOUND ( 'NONE', #383, .T. ) ;
#12895 = ORIENTED_EDGE ( 'NONE', *, *, #6410, .T. ) ;
#12896 = ORIENTED_EDGE ( 'NONE', *, *, #5298, .T. ) ;
#12897 = CYLINDRICAL_SURFACE ( 'NONE', #2850, 0.7366000000000039183 ) ;
#12898 = ORIENTED_EDGE ( 'NONE', *, *, #3326, .T. ) ;
#12899 =( NAMED_UNIT ( * ) SI_UNIT ( $, .STERADIAN. ) SOLID_ANGLE_UNIT ( ) );
#12900 = ORIENTED_EDGE ( 'NONE', *, *, #8752, .F. ) ;
#12901 = AXIS2_PLACEMENT_3D ( 'NONE', #7893, #6510, #11766 ) ;
#12902 = ORIENTED_EDGE ( 'NONE', *, *, #16907, .F. ) ;
#12903 = DIRECTION ( 'NONE',  ( 0.000000000000000000, 0.000000000000000000, 1.000000000000000000 ) ) ;
#12904 = LINE ( 'NONE', #9043, #7224 ) ;
#12905 = EDGE_LOOP ( 'NONE', ( #6393, #10074, #3659, #13800 ) ) ;
#12906 = CARTESIAN_POINT ( 'NONE',  ( -440.0000000000000568, 620.7506394335853201, -11.00000000000000000 ) ) ;
#12907 = EDGE_CURVE ( 'NONE', #14070, #2365, #10366, .T. ) ;
#12908 = CARTESIAN_POINT ( 'NONE',  ( -26.00000000000002842, 3.000000000000000000, -31.00000000000003197 ) ) ;
#12909 = ORIENTED_EDGE ( 'NONE', *, *, #10358, .T. ) ;
#12910 = CARTESIAN_POINT ( 'NONE',  ( 40.00000000000000000, 68.00000000000000000, -25.99999999999999645 ) ) ;
#12911 = DIRECTION ( 'NONE',  ( -1.000000000000000000, 0.000000000000000000, 1.196361017915039732E-16 ) ) ;
#12912 = EDGE_LOOP ( 'NONE', ( #13055, #14533, #1816, #12781 ) ) ;
#12913 = AXIS2_PLACEMENT_3D ( 'NONE', #9428, #3070, #13558 ) ;
#12914 = EDGE_CURVE ( 'NONE', #3292, #9705, #13988, .T. ) ;
#12915 = DIRECTION ( 'NONE',  ( -0.000000000000000000, -1.000000000000000000, -0.000000000000000000 ) ) ;
#12916 = ORIENTED_EDGE ( 'NONE', *, *, #10893, .F. ) ;
#12917 = CARTESIAN_POINT ( 'NONE',  ( 17.99999999999998224, 6.000000000000000000, -35.99999999999999289 ) ) ;
#12918 = EDGE_LOOP ( 'NONE', ( #3797, #16597 ) ) ;
#12919 = ORIENTED_EDGE ( 'NONE', *, *, #9608, .F. ) ;
#12920 = DIRECTION ( 'NONE',  ( 0.000000000000000000, 0.000000000000000000, -1.000000000000000000 ) ) ;
#12921 = PRODUCT_RELATED_PRODUCT_CATEGORY ( 'part', '', ( #9625 ) ) ;
#12922 = DIRECTION ( 'NONE',  ( 0.000000000000000000, -1.000000000000000000, 0.000000000000000000 ) ) ;
#12923 = CARTESIAN_POINT ( 'NONE',  ( -22.00000000000001776, 8.000000000000000000, 33.00000000000000711 ) ) ;
#12924 = VECTOR ( 'NONE', #4589, 1000.000000000000000 ) ;
#12925 = ORIENTED_EDGE ( 'NONE', *, *, #11404, .F. ) ;
#12926 = FACE_OUTER_BOUND ( 'NONE', #15901, .T. ) ;
#12927 = DIRECTION ( 'NONE',  ( 0.000000000000000000, -1.000000000000000000, 0.000000000000000000 ) ) ;
#12928 = ADVANCED_FACE ( 'NONE', ( #11472 ), #2286, .T. ) ;
#12929 = LINE ( 'NONE', #7516, #12349 ) ;
#12930 = CLOSED_SHELL ( 'NONE', ( #11736, #9314, #2793, #1314, #15977, #10141, #9760, #975, #7416, #13868, #16100, #10963, #45, #1633, #2995, #10702, #3785, #5184 ) ) ;
#12931 = MECHANICAL_DESIGN_GEOMETRIC_PRESENTATION_REPRESENTATION (  '', ( #14041 ), #6612 ) ;
#12932 = LINE ( 'NONE', #14059, #3752 ) ;
#12933 = DIRECTION ( 'NONE',  ( 0.000000000000000000, 0.000000000000000000, 1.000000000000000000 ) ) ;
#12934 = CARTESIAN_POINT ( 'NONE',  ( 3.500000000000000000, -18.50000000000000000, -2.265596578422603396E-15 ) ) ;
#12935 = CYLINDRICAL_SURFACE ( 'NONE', #12345, 0.7365999999987759006 ) ;
#12937 = ORIENTED_EDGE ( 'NONE', *, *, #6022, .T. ) ;
#12936 = ORIENTED_EDGE ( 'NONE', *, *, #6556, .T. ) ;
#12938 = AXIS2_PLACEMENT_3D ( 'NONE', #13756, #12726, #4724 ) ;
#12939 = DIRECTION ( 'NONE',  ( -1.000000000000000000, -0.000000000000000000, -0.000000000000000000 ) ) ;
#12940 = AXIS2_PLACEMENT_3D ( 'NONE', #4203, #6768, #8228 ) ;
#12941 = DIRECTION ( 'NONE',  ( 0.000000000000000000, 0.000000000000000000, -1.000000000000000000 ) ) ;
#12942 = ADVANCED_FACE ( 'NONE', ( #9069 ), #16957, .T. ) ;
#12943 = VECTOR ( 'NONE', #6932, 1000.000000000000000 ) ;
#12944 = AXIS2_PLACEMENT_3D ( 'NONE', #8915, #9072, #12933 ) ;
#12945 = AXIS2_PLACEMENT_3D ( 'NONE', #15796, #15626, #14341 ) ;
#12946 = LINE ( 'NONE', #1024, #10493 ) ;
#12947 = ORIENTED_EDGE ( 'NONE', *, *, #5502, .F. ) ;
#12948 = DIRECTION ( 'NONE',  ( 0.000000000000000000, 0.000000000000000000, -1.000000000000000000 ) ) ;
#12949 = ADVANCED_FACE ( 'NONE', ( #5186 ), #15597, .T. ) ;
#12950 = CARTESIAN_POINT ( 'NONE',  ( 39.75350601975127063, 301.2117639810886089, -6.736600000000000144 ) ) ;
#12951 = VERTEX_POINT ( 'NONE', #11731 ) ;
#12952 = CARTESIAN_POINT ( 'NONE',  ( 45.00000000000000000, 473.6663340069157471, -517.8058340126048051 ) ) ;
#12953 = LINE ( 'NONE', #1191, #2700 ) ;
#12954 = CARTESIAN_POINT ( 'NONE',  ( -5.000000000000000888, 0.000000000000000000, 0.000000000000000000 ) ) ;
#12955 = VERTEX_POINT ( 'NONE', #4940 ) ;
#12956 = DIRECTION ( 'NONE',  ( 1.000000000000000000, 0.000000000000000000, 0.000000000000000000 ) ) ;
#12957 = VECTOR ( 'NONE', #13409, 1000.000000000000000 ) ;
#12958 = DIRECTION ( 'NONE',  ( 1.000000000000000000, -0.000000000000000000, -0.000000000000000000 ) ) ;
#12959 = CARTESIAN_POINT ( 'NONE',  ( 45.00000000000000000, 493.2350855268086320, -494.4847040861889127 ) ) ;
#12960 = EDGE_LOOP ( 'NONE', ( #15265, #2138, #10586, #16065 ) ) ;
#12961 = CYLINDRICAL_SURFACE ( 'NONE', #4515, 5.000000000000000888 ) ;
#12962 = SHAPE_REPRESENTATION ( 'Part8', ( #1488 ), #16580 ) ;
#12963 = CONTEXT_DEPENDENT_SHAPE_REPRESENTATION ( #14339, #15761 ) ;
#12964 = VECTOR ( 'NONE', #13211, 1000.000000000000000 ) ;
#12965 = DIRECTION ( 'NONE',  ( 1.000000000000000000, 0.000000000000000000, 0.000000000000000000 ) ) ;
#12966 = EDGE_CURVE ( 'NONE', #2788, #1418, #12929, .T. ) ;
#12967 = DIRECTION ( 'NONE',  ( 1.000000000000000000, -0.000000000000000000, 0.000000000000000000 ) ) ;
#12968 = ORIENTED_EDGE ( 'NONE', *, *, #829, .F. ) ;
#12969 = AXIS2_PLACEMENT_3D ( 'NONE', #6841, #5393, #9350 ) ;
#12970 = VECTOR ( 'NONE', #2396, 1000.000000000000000 ) ;
#12971 = AXIS2_PLACEMENT_3D ( 'NONE', #12923, #6380, #16872 ) ;
#12972 = CARTESIAN_POINT ( 'NONE',  ( 10.00000000000000000, 620.7506394335853201, 0.000000000000000000 ) ) ;
#12973 = ADVANCED_FACE ( 'NONE', ( #10192 ), #11551, .F. ) ;
#12974 = DIRECTION ( 'NONE',  ( -0.000000000000000000, -1.000000000000000000, -0.000000000000000000 ) ) ;
#12975 = ADVANCED_FACE ( 'NONE', ( #2200 ), #1167, .T. ) ;
#12976 = EDGE_CURVE ( 'NONE', #9819, #3376, #6146, .T. ) ;
#12977 = DIRECTION ( 'NONE',  ( -1.000000000000000000, -1.672079375435207996E-12, 1.507226479265539607E-13 ) ) ;
#12978 = ORIENTED_EDGE ( 'NONE', *, *, #1855, .F. ) ;
#12979 = CARTESIAN_POINT ( 'NONE',  ( -37.00000000000000711, 6.000000000000000000, -18.00000000000000355 ) ) ;
#12980 = EDGE_CURVE ( 'NONE', #9616, #13962, #8511, .T. ) ;
#12981 = LINE ( 'NONE', #7980, #15285 ) ;
#12982 = EDGE_LOOP ( 'NONE', ( #14800, #3529, #942, #11894 ) ) ;
#12983 = VECTOR ( 'NONE', #10167, 1000.000000000000000 ) ;
#12984 = DIRECTION ( 'NONE',  ( 1.000000000000000000, -0.000000000000000000, 0.000000000000000000 ) ) ;
#12985 = ORIENTED_EDGE ( 'NONE', *, *, #4784, .F. ) ;
#12986 = VERTEX_POINT ( 'NONE', #15428 ) ;
#12987 = VECTOR ( 'NONE', #12832, 1000.000000000000000 ) ;
#12988 = LINE ( 'NONE', #5233, #8069 ) ;
#12989 = AXIS2_PLACEMENT_3D ( 'NONE', #9158, #11549, #6383 ) ;
#12990 = VECTOR ( 'NONE', #3052, 1000.000000000000000 ) ;
#12991 = VERTEX_POINT ( 'NONE', #16631 ) ;
#12992 = SHAPE_REPRESENTATION_RELATIONSHIP ( 'NONE' , 'NONE' ,  #7676, #12618 ) ;
#12993 = ORIENTED_EDGE ( 'NONE', *, *, #4546, .T. ) ;
#12994 = CIRCLE ( 'NONE', #5309, 4.695405383896011919 ) ;
#12995 = ORIENTED_EDGE ( 'NONE', *, *, #11561, .F. ) ;
#12996 = LINE ( 'NONE', #3806, #11294 ) ;
#12997 = PLANE ( 'NONE',  #14650 ) ;
#12998 = VECTOR ( 'NONE', #802, 1000.000000000000000 ) ;
#12999 = AXIS2_PLACEMENT_3D ( 'NONE', #9662, #5438, #555 ) ;
#13000 = ORIENTED_EDGE ( 'NONE', *, *, #11255, .T. ) ;
#13001 = DIRECTION ( 'NONE',  ( 0.000000000000000000, 1.000000000000000000, 0.000000000000000000 ) ) ;
#13002 = ADVANCED_FACE ( 'NONE', ( #11647 ), #4864, .F. ) ;
#13003 = AXIS2_PLACEMENT_3D ( 'NONE', #4236, #10846, #6877 ) ;
#13004 = CIRCLE ( 'NONE', #399, 13.69540538389601991 ) ;
#13005 = CARTESIAN_POINT ( 'NONE',  ( 39.06972645625037899, 346.7108172824755457, -6.736600000000000144 ) ) ;
#13006 = EDGE_LOOP ( 'NONE', ( #11981, #15427, #10765, #6608 ) ) ;
#13007 = CARTESIAN_POINT ( 'NONE',  ( -45.00000000000000000, 473.6663340069157471, -517.8058340126048051 ) ) ;
#13008 = CARTESIAN_POINT ( 'NONE',  ( 10.00000000000000000, 425.7506394335853201, -11.00000000000000000 ) ) ;
#13009 = CIRCLE ( 'NONE', #14097, 5.268482129199949959 ) ;
#13010 = ORIENTED_EDGE ( 'NONE', *, *, #3295, .F. ) ;
#13011 = CARTESIAN_POINT ( 'NONE',  ( -34.99999999999996447, 0.000000000000000000, -40.00000000000000711 ) ) ;
#13012 = ORIENTED_EDGE ( 'NONE', *, *, #4663, .T. ) ;
#13013 = CARTESIAN_POINT ( 'NONE',  ( 0.000000000000000000, 1.106257942394396377E-12, -155.0000000000060254 ) ) ;
#13014 = PRODUCT_DEFINITION_FORMATION_WITH_SPECIFIED_SOURCE ( 'ANY', '', #9040, .NOT_KNOWN. ) ;
#13015 = AXIS2_PLACEMENT_3D ( 'NONE', #6257, #7714, #11508 ) ;
#13016 = ORIENTED_EDGE ( 'NONE', *, *, #4733, .F. ) ;
#13017 = EDGE_CURVE ( 'NONE', #8178, #16566, #8912, .T. ) ;
#13018 = EDGE_LOOP ( 'NONE', ( #3178, #14639, #43, #13860, #14452 ) ) ;
#13019 = FACE_OUTER_BOUND ( 'NONE', #1162, .T. ) ;
#13020 = VECTOR ( 'NONE', #9887, 1000.000000000000000 ) ;
#13021 = DIRECTION ( 'NONE',  ( 0.000000000000000000, 1.000000000000000000, 0.000000000000000000 ) ) ;
#13022 = LINE ( 'NONE', #1595, #9153 ) ;
#13023 = EDGE_LOOP ( 'NONE', ( #1928, #10431, #2670, #1666 ) ) ;
#13024 = CARTESIAN_POINT ( 'NONE',  ( 0.000000000000000000, 336.2713855965630501, -311.0652884549417081 ) ) ;
#13025 = PRODUCT ( 'Servo-Body', 'Servo-Body', '', ( #6088 ) ) ;
#13026 = DIRECTION ( 'NONE',  ( -1.000000000000000000, 0.000000000000000000, 0.000000000000000000 ) ) ;
#13027 = DIRECTION ( 'NONE',  ( 0.000000000000000000, 0.000000000000000000, -1.000000000000000000 ) ) ;
#13028 = DIRECTION ( 'NONE',  ( -0.000000000000000000, -1.000000000000000000, -0.000000000000000000 ) ) ;
#13029 = DIRECTION ( 'NONE',  ( 1.000000000000000000, 0.000000000000000000, 0.000000000000000000 ) ) ;
#13030 = CARTESIAN_POINT ( 'NONE',  ( 35.00000000000003553, 0.000000000000000000, -20.99999999999999645 ) ) ;
#13031 = VECTOR ( 'NONE', #2378, 1000.000000000000227 ) ;
#13032 = CARTESIAN_POINT ( 'NONE',  ( 31.00000000000001421, 0.000000000000000000, 22.99999999999999645 ) ) ;
#13033 = CARTESIAN_POINT ( 'NONE',  ( -34.99999999999998579, 0.000000000000000000, 18.50000000000000355 ) ) ;
#13034 = CIRCLE ( 'NONE', #693, 5.000000000000004441 ) ;
#13036 = ORIENTED_EDGE ( 'NONE', *, *, #8869, .F. ) ;
#13035 = ORIENTED_EDGE ( 'NONE', *, *, #10397, .T. ) ;
#13037 = DIRECTION ( 'NONE',  ( 0.000000000000000000, 1.000000000000000000, 0.000000000000000000 ) ) ;
#13038 = EDGE_CURVE ( 'NONE', #8101, #3466, #2718, .T. ) ;
#13039 = CARTESIAN_POINT ( 'NONE',  ( 10.00000000000000000, 185.0000000000000000, -486.7326477857670852 ) ) ;
#13040 = CARTESIAN_POINT ( 'NONE',  ( -33.00000000000000000, 8.000000000000000000, -26.00000000000000355 ) ) ;
#13041 = CARTESIAN_POINT ( 'NONE',  ( 0.000000000000000000, 309.2289037985885898, -83.18019484660915452 ) ) ;
#13042 = ORIENTED_EDGE ( 'NONE', *, *, #11192, .F. ) ;
#13043 = VECTOR ( 'NONE', #1687, 1000.000000000000000 ) ;
#13044 = DIRECTION ( 'NONE',  ( -1.000000000000000000, -0.000000000000000000, -0.000000000000000000 ) ) ;
#13045 = DIRECTION ( 'NONE',  ( -1.000000000000000000, 0.000000000000000000, -0.000000000000000000 ) ) ;
#13046 = ORIENTED_EDGE ( 'NONE', *, *, #5576, .T. ) ;
#13047 = DIRECTION ( 'NONE',  ( 0.000000000000000000, 0.9161352426163912321, -0.4008693268837190127 ) ) ;
#13048 = DIRECTION ( 'NONE',  ( 0.000000000000000000, -1.000000000000000000, -1.321694076934710402E-16 ) ) ;
#13049 = DIRECTION ( 'NONE',  ( 0.000000000000000000, 0.000000000000000000, 1.000000000000000000 ) ) ;
#13050 = ORIENTED_EDGE ( 'NONE', *, *, #2015, .F. ) ;
#13051 = EDGE_CURVE ( 'NONE', #16546, #14070, #15764, .T. ) ;
#13052 = LINE ( 'NONE', #14174, #5195 ) ;
#13053 = CYLINDRICAL_SURFACE ( 'NONE', #16118, 4.999999999999997335 ) ;
#13054 = CARTESIAN_POINT ( 'NONE',  ( 35.00000000000000711, 19.00000000000000000, 20.99999999999999289 ) ) ;
#13055 = ORIENTED_EDGE ( 'NONE', *, *, #7866, .T. ) ;
#13056 = ADVANCED_BREP_SHAPE_REPRESENTATION ( '', ( #8355, #1488 ), #5871 ) ;
#13057 = VECTOR ( 'NONE', #4821, 1000.000000000000000 ) ;
#13058 = DIRECTION ( 'NONE',  ( -0.000000000000000000, -1.000000000000000000, -0.000000000000000000 ) ) ;
#13059 = CIRCLE ( 'NONE', #16341, 7.500000000000007105 ) ;
#13060 = ITEM_DEFINED_TRANSFORMATION ( 'NONE', 'NONE', #4509,  #1488 ) ;
#13061 = EDGE_CURVE ( 'NONE', #10961, #6790, #11994, .T. ) ;
#13062 =( LENGTH_UNIT ( ) NAMED_UNIT ( * ) SI_UNIT ( .MILLI., .METRE. ) );
#13063 = CARTESIAN_POINT ( 'NONE',  ( 46.99999999999988631, 549.5810598491749488, -575.3306267969850296 ) ) ;
#13064 = EDGE_LOOP ( 'NONE', ( #761, #13345, #10816, #7 ) ) ;
#13065 = DIRECTION ( 'NONE',  ( -1.000000000000000000, 0.000000000000000000, 0.000000000000000000 ) ) ;
#13066 = CARTESIAN_POINT ( 'NONE',  ( 1.050000000000000044, 15.25000000000000000, 0.000000000000000000 ) ) ;
#13067 = AXIS2_PLACEMENT_3D ( 'NONE', #6166, #780, #7114 ) ;
#13068 = DIRECTION ( 'NONE',  ( -1.000000000000000000, -0.000000000000000000, -0.000000000000000000 ) ) ;
#13069 = ORIENTED_EDGE ( 'NONE', *, *, #11704, .F. ) ;
#13070 = CIRCLE ( 'NONE', #5926, 25.25038683781155413 ) ;
#13071 = PLANE ( 'NONE',  #6126 ) ;
#13072 = CARTESIAN_POINT ( 'NONE',  ( -35.00000000000000000, 8.000000000000000000, -21.00000000000000000 ) ) ;
#13073 = VERTEX_POINT ( 'NONE', #5631 ) ;
#13074 = EDGE_CURVE ( 'NONE', #16546, #15577, #8029, .T. ) ;
#13075 = CARTESIAN_POINT ( 'NONE',  ( -31.00000000000000000, 8.000000000000000000, 30.99999999999999289 ) ) ;
#13076 = VERTEX_POINT ( 'NONE', #2794 ) ;
#13077 = ORIENTED_EDGE ( 'NONE', *, *, #11477, .F. ) ;
#13078 = CARTESIAN_POINT ( 'NONE',  ( 31.00000000000002842, 0.000000000000000000, 23.00000000000001066 ) ) ;
#13079 = ORIENTED_EDGE ( 'NONE', *, *, #14643, .T. ) ;
#13080 = EDGE_CURVE ( 'NONE', #9920, #5349, #16194, .T. ) ;
#13081 = VECTOR ( 'NONE', #13199, 1000.000000000000000 ) ;
#13082 = ADVANCED_FACE ( 'NONE', ( #11814 ), #7939, .F. ) ;
#13083 = EDGE_CURVE ( 'NONE', #8729, #16870, #4353, .T. ) ;
#13084 = ORIENTED_EDGE ( 'NONE', *, *, #7567, .F. ) ;
#13085 = VERTEX_POINT ( 'NONE', #14661 ) ;
#13086 = DIRECTION ( 'NONE',  ( 1.000000000000000000, -0.000000000000000000, -0.000000000000000000 ) ) ;
#13087 = FACE_OUTER_BOUND ( 'NONE', #6307, .T. ) ;
#13088 = VERTEX_POINT ( 'NONE', #9328 ) ;
#13089 = DIRECTION ( 'NONE',  ( 1.000000000000000000, -0.000000000000000000, 0.000000000000000000 ) ) ;
#13090 = DIRECTION ( 'NONE',  ( 0.000000000000000000, 0.000000000000000000, 1.000000000000000000 ) ) ;
#13091 = CIRCLE ( 'NONE', #7316, 4.999999999999997335 ) ;
#13092 = LINE ( 'NONE', #12908, #1736 ) ;
#13093 = VERTEX_POINT ( 'NONE', #2710 ) ;
#13094 = DIRECTION ( 'NONE',  ( -0.000000000000000000, 1.000000000000000000, -0.000000000000000000 ) ) ;
#13095 = DIRECTION ( 'NONE',  ( 1.000000000000000000, -0.000000000000000000, -0.000000000000000000 ) ) ;
#13096 = ORIENTED_EDGE ( 'NONE', *, *, #15672, .T. ) ;
#13097 = DIRECTION ( 'NONE',  ( 0.000000000000000000, 0.000000000000000000, 1.000000000000000000 ) ) ;
#13098 = ORIENTED_EDGE ( 'NONE', *, *, #9295, .F. ) ;
#13099 = EDGE_CURVE ( 'NONE', #971, #4249, #13288, .T. ) ;
#13100 = EDGE_CURVE ( 'NONE', #3987, #1755, #147, .T. ) ;
#13101 = CARTESIAN_POINT ( 'NONE',  ( 37.18009836720080585, 275.4439001176564830, 0.000000000000000000 ) ) ;
#13102 = EDGE_CURVE ( 'NONE', #16324, #5761, #8122, .T. ) ;
#13103 = ORIENTED_EDGE ( 'NONE', *, *, #16531, .F. ) ;
#13104 = CONICAL_SURFACE ( 'NONE', #8718, 12.32407335584850117, 0.8899833664651138898 ) ;
#13105 = ORIENTED_EDGE ( 'NONE', *, *, #11588, .F. ) ;
#13106 = DIRECTION ( 'NONE',  ( 0.000000000000000000, 0.000000000000000000, 1.000000000000000000 ) ) ;
#13107 = DIRECTION ( 'NONE',  ( 0.000000000000000000, 0.000000000000000000, -1.000000000000000000 ) ) ;
#13108 = FACE_OUTER_BOUND ( 'NONE', #9041, .T. ) ;
#13109 = ORIENTED_EDGE ( 'NONE', *, *, #2696, .F. ) ;
#13110 = PLANE ( 'NONE',  #612 ) ;
#13111 = CARTESIAN_POINT ( 'NONE',  ( 10.00000000000000000, 341.0487089519837696, -115.0000000000032969 ) ) ;
#13112 = DIRECTION ( 'NONE',  ( 1.000000000000000000, 0.000000000000000000, 0.000000000000000000 ) ) ;
#13113 = FACE_BOUND ( 'NONE', #10580, .T. ) ;
#13114 = DIRECTION ( 'NONE',  ( -1.000000000000000000, -0.000000000000000000, -0.000000000000000000 ) ) ;
#13115 = CIRCLE ( 'NONE', #6562, 13.69540538389601991 ) ;
#13116 = DIRECTION ( 'NONE',  ( 1.000000000000000000, 0.000000000000000000, -0.000000000000000000 ) ) ;
#13117 = VECTOR ( 'NONE', #16184, 1000.000000000000000 ) ;
#13118 = FACE_OUTER_BOUND ( 'NONE', #16370, .T. ) ;
#13120 = ORIENTED_EDGE ( 'NONE', *, *, #6870, .F. ) ;
#13119 = ORIENTED_EDGE ( 'NONE', *, *, #5501, .T. ) ;
#13121 = CARTESIAN_POINT ( 'NONE',  ( 0.000000000000000000, 185.0000000000000000, -486.7326477857670852 ) ) ;
#13122 = DIRECTION ( 'NONE',  ( 6.123031769111888756E-17, 0.000000000000000000, 1.000000000000000000 ) ) ;
#13123 = CARTESIAN_POINT ( 'NONE',  ( 415.0210210471910841, 329.6061121441327941, 0.000000000000000000 ) ) ;
#13124 = FACE_OUTER_BOUND ( 'NONE', #3802, .T. ) ;
#13125 = ORIENTED_EDGE ( 'NONE', *, *, #16926, .F. ) ;
#13126 = AXIS2_PLACEMENT_3D ( 'NONE', #316, #6985, #3058 ) ;
#13127 = CARTESIAN_POINT ( 'NONE',  ( 21.00000000000000000, 8.000000000000000000, -35.00000000000000711 ) ) ;
#13128 = LINE ( 'NONE', #12866, #1830 ) ;
#13129 = ORIENTED_EDGE ( 'NONE', *, *, #12907, .F. ) ;
#13130 = DIRECTION ( 'NONE',  ( 1.000000000000000000, -0.000000000000000000, -0.000000000000000000 ) ) ;
#13131 = ADVANCED_FACE ( 'NONE', ( #1338 ), #5271, .F. ) ;
#13132 = DIRECTION ( 'NONE',  ( -0.9740972002433518906, 0.2261297071993489949, 0.000000000000000000 ) ) ;
#13133 = DIRECTION ( 'NONE',  ( -0.000000000000000000, -1.000000000000000000, 0.000000000000000000 ) ) ;
#13134 = CARTESIAN_POINT ( 'NONE',  ( 49.99999999999999289, 515.4878487013597805, -631.7230258972047068 ) ) ;
#13135 = FACE_OUTER_BOUND ( 'NONE', #5764, .T. ) ;
#13136 = EDGE_LOOP ( 'NONE', ( #16502, #5207, #2576, #14108 ) ) ;
#13137 = DIRECTION ( 'NONE',  ( 0.000000000000000000, 0.000000000000000000, 1.000000000000000000 ) ) ;
#13138 = SHAPE_REPRESENTATION_RELATIONSHIP ( 'NONE' , 'NONE' ,  #7583, #13056 ) ;
#13139 = CARTESIAN_POINT ( 'NONE',  ( 10.00000000000000000, 0.000000000000000000, 0.000000000000000000 ) ) ;
#13140 = VECTOR ( 'NONE', #4751, 1000.000000000000000 ) ;
#13141 = ORIENTED_EDGE ( 'NONE', *, *, #801, .T. ) ;
#13142 = PRODUCT_DEFINITION ( 'UNKNOWN', '', #10820, #13581 ) ;
#13143 = FACE_OUTER_BOUND ( 'NONE', #11172, .T. ) ;
#13144 = FACE_OUTER_BOUND ( 'NONE', #10581, .T. ) ;
#13145 = DIRECTION ( 'NONE',  ( 0.000000000000000000, 0.000000000000000000, 1.000000000000000000 ) ) ;
#13146 = ORIENTED_EDGE ( 'NONE', *, *, #10767, .F. ) ;
#13147 = CARTESIAN_POINT ( 'NONE',  ( 1.250085104875786612E-12, 220.0768326692952996, 286.9685381829922903 ) ) ;
#13148 = DIRECTION ( 'NONE',  ( 0.000000000000000000, 1.000000000000000000, 0.000000000000000000 ) ) ;
#13149 = CARTESIAN_POINT ( 'NONE',  ( 0.000000000000000000, 23.00000000000000000, 0.000000000000000000 ) ) ;
#13150 = ORIENTED_EDGE ( 'NONE', *, *, #12700, .F. ) ;
#13151 = EDGE_CURVE ( 'NONE', #6787, #3377, #6302, .T. ) ;
#13152 = DIRECTION ( 'NONE',  ( -0.000000000000000000, 1.000000000000000000, -0.000000000000000000 ) ) ;
#13153 = ORIENTED_EDGE ( 'NONE', *, *, #14624, .T. ) ;
#13154 = ORIENTED_EDGE ( 'NONE', *, *, #2477, .F. ) ;
#13155 = AXIS2_PLACEMENT_3D ( 'NONE', #6849, #5572, #10821 ) ;
#13156 = CARTESIAN_POINT ( 'NONE',  ( -22.99999999999999645, 68.00000000000000000, 37.00000000000002132 ) ) ;
#13157 = ORIENTED_EDGE ( 'NONE', *, *, #14744, .T. ) ;
#13158 = EDGE_LOOP ( 'NONE', ( #5413, #3753, #16673, #8875 ) ) ;
#13159 =( NAMED_UNIT ( * ) PLANE_ANGLE_UNIT ( ) SI_UNIT ( $, .RADIAN. ) );
#13160 = ORIENTED_EDGE ( 'NONE', *, *, #5174, .T. ) ;
#13161 = ORIENTED_EDGE ( 'NONE', *, *, #90, .T. ) ;
#13162 = EDGE_CURVE ( 'NONE', #2814, #15921, #1348, .T. ) ;
#13163 = ADVANCED_FACE ( 'NONE', ( #13197 ), #9504, .F. ) ;
#13164 = FACE_OUTER_BOUND ( 'NONE', #2940, .T. ) ;
#13165 = DIRECTION ( 'NONE',  ( -1.000000000000000000, 0.000000000000000000, 0.000000000000000000 ) ) ;
#13166 = VECTOR ( 'NONE', #6306, 1000.000000000000000 ) ;
#13167 = EDGE_LOOP ( 'NONE', ( #8185, #8397, #14980, #8565 ) ) ;
#13169 = CARTESIAN_POINT ( 'NONE',  ( -22.00000000000001776, 8.000000000000000000, 36.00000000000000711 ) ) ;
#13168 = AXIS2_PLACEMENT_3D ( 'NONE', #16707, #12850, #7426 ) ;
#13170 = EDGE_CURVE ( 'NONE', #16075, #1644, #5368, .T. ) ;
#13171 = CARTESIAN_POINT ( 'NONE',  ( -37.00000000000000711, 10.00000000000000000, 23.00000000000000000 ) ) ;
#13172 = ORIENTED_EDGE ( 'NONE', *, *, #15398, .F. ) ;
#13173 = EDGE_CURVE ( 'NONE', #16404, #2588, #7916, .T. ) ;
#13174 = EDGE_CURVE ( 'NONE', #750, #7474, #6266, .T. ) ;
#13175 = DIRECTION ( 'NONE',  ( 1.000000000000000000, 0.000000000000000000, 0.000000000000000000 ) ) ;
#13176 = ORIENTED_EDGE ( 'NONE', *, *, #879, .F. ) ;
#13177 = CARTESIAN_POINT ( 'NONE',  ( 21.99999999999998224, 10.00000000000000000, -32.99999999999999289 ) ) ;
#13178 = FACE_OUTER_BOUND ( 'NONE', #9512, .T. ) ;
#13179 = ORIENTED_EDGE ( 'NONE', *, *, #5744, .T. ) ;
#13180 = FACE_OUTER_BOUND ( 'NONE', #8640, .T. ) ;
#13181 = ORIENTED_EDGE ( 'NONE', *, *, #7679, .T. ) ;
#13182 = DIRECTION ( 'NONE',  ( 0.000000000000000000, 0.000000000000000000, -1.000000000000000000 ) ) ;
#13183 = AXIS2_PLACEMENT_3D ( 'NONE', #14383, #7842, #13097 ) ;
#13184 = ORIENTED_EDGE ( 'NONE', *, *, #10040, .T. ) ;
#13185 = VERTEX_POINT ( 'NONE', #2969 ) ;
#13186 = SURFACE_SIDE_STYLE ('',( #6730 ) ) ;
#13187 = EDGE_CURVE ( 'NONE', #7379, #594, #8203, .T. ) ;
#13188 = AXIS2_PLACEMENT_3D ( 'NONE', #8843, #1194, #6411 ) ;
#13189 = CARTESIAN_POINT ( 'NONE',  ( 0.000000000000000000, 284.6994879831845537, 28.46994879831456515 ) ) ;
#13190 = ORIENTED_EDGE ( 'NONE', *, *, #5476, .F. ) ;
#13191 = CARTESIAN_POINT ( 'NONE',  ( -31.81980515339462912, 0.000000000000000000, 28.51980515339464972 ) ) ;
#13192 = DIRECTION ( 'NONE',  ( 0.000000000000000000, 1.000000000000000000, 0.000000000000000000 ) ) ;
#13193 = ADVANCED_FACE ( 'NONE', ( #9677 ), #8465, .F. ) ;
#13194 = EDGE_CURVE ( 'NONE', #11595, #5928, #14513, .T. ) ;
#13195 = AXIS2_PLACEMENT_3D ( 'NONE', #12509, #3576, #7592 ) ;
#13196 = ADVANCED_FACE ( 'NONE', ( #14995 ), #11204, .T. ) ;
#13197 = FACE_OUTER_BOUND ( 'NONE', #10394, .T. ) ;
#13198 = EDGE_CURVE ( 'NONE', #11402, #2493, #9918, .T. ) ;
#13199 = DIRECTION ( 'NONE',  ( 8.659560562354968603E-17, 0.7071067811865445751, -0.7071067811865504593 ) ) ;
#13200 = DIRECTION ( 'NONE',  ( 0.000000000000000000, 0.000000000000000000, -1.000000000000000000 ) ) ;
#13201 = DIRECTION ( 'NONE',  ( 0.000000000000000000, 0.9950371902099902632, -0.09950371902098713306 ) ) ;
#13202 = SURFACE_SIDE_STYLE ('',( #3062 ) ) ;
#13204 = ORIENTED_EDGE ( 'NONE', *, *, #16683, .F. ) ;
#13203 = ORIENTED_EDGE ( 'NONE', *, *, #8092, .T. ) ;
#13205 = DIRECTION ( 'NONE',  ( 1.000000000000000000, 0.000000000000000000, 0.000000000000000000 ) ) ;
#13206 = VECTOR ( 'NONE', #16602, 1000.000000000000000 ) ;
#13207 = FACE_OUTER_BOUND ( 'NONE', #2428, .T. ) ;
#13208 = DIRECTION ( 'NONE',  ( 0.000000000000000000, -1.000000000000000000, 0.000000000000000000 ) ) ;
#13209 = FACE_OUTER_BOUND ( 'NONE', #13018, .T. ) ;
#13210 = ORIENTED_EDGE ( 'NONE', *, *, #8043, .F. ) ;
#13211 = DIRECTION ( 'NONE',  ( -0.000000000000000000, -0.000000000000000000, 1.000000000000000000 ) ) ;
#13212 = CARTESIAN_POINT ( 'NONE',  ( 35.00000000000000711, 11.00000000000000000, 35.00000000000000711 ) ) ;
#13213 = VERTEX_POINT ( 'NONE', #5794 ) ;
#13214 = DIRECTION ( 'NONE',  ( 0.000000000000000000, 0.000000000000000000, 1.000000000000000000 ) ) ;
#13215 = EDGE_CURVE ( 'NONE', #12955, #11618, #10163, .T. ) ;
#13216 = DIRECTION ( 'NONE',  ( -0.000000000000000000, -1.000000000000000000, 0.000000000000000000 ) ) ;
#13217 = ORIENTED_EDGE ( 'NONE', *, *, #686, .F. ) ;
#13218 = CIRCLE ( 'NONE', #6607, 9.000000000000007105 ) ;
#13219 = DIRECTION ( 'NONE',  ( 0.000000000000000000, 0.000000000000000000, -1.000000000000000000 ) ) ;
#13220 = DIRECTION ( 'NONE',  ( 0.000000000000000000, 0.5150380749100629263, 0.8571673007021070045 ) ) ;
#13221 = ORIENTED_EDGE ( 'NONE', *, *, #12765, .F. ) ;
#13222 = AXIS2_PLACEMENT_3D ( 'NONE', #16901, #1364, #9096 ) ;
#13223 = DIRECTION ( 'NONE',  ( -1.000000000000000000, -0.000000000000000000, -0.000000000000000000 ) ) ;
#13224 = AXIS2_PLACEMENT_3D ( 'NONE', #4451, #16213, #5390 ) ;
#13225 = AXIS2_PLACEMENT_3D ( 'NONE', #3489, #14922, #3165 ) ;
#13226 = DIRECTION ( 'NONE',  ( 0.000000000000000000, 0.000000000000000000, -1.000000000000000000 ) ) ;
#13227 = EDGE_CURVE ( 'NONE', #3880, #15603, #8490, .T. ) ;
#13228 = DIRECTION ( 'NONE',  ( -0.000000000000000000, -1.000000000000000000, 0.000000000000000000 ) ) ;
#13229 = CIRCLE ( 'NONE', #77, 0.6999999999999992895 ) ;
#13230 = ORIENTED_EDGE ( 'NONE', *, *, #5056, .T. ) ;
#13231 = CARTESIAN_POINT ( 'NONE',  ( 0.000000000000000000, 0.000000000000000000, 0.000000000000000000 ) ) ;
#13232 = UNCERTAINTY_MEASURE_WITH_UNIT (LENGTH_MEASURE( 1.000000000000000082E-05 ), #11724, 'distance_accuracy_value', 'NONE');
#13233 = DIRECTION ( 'NONE',  ( 0.000000000000000000, 0.000000000000000000, -1.000000000000000000 ) ) ;
#13234 = CARTESIAN_POINT ( 'NONE',  ( -23.00000000000002487, 10.00000000000000000, -31.00000000000003553 ) ) ;
#13235 = ORIENTED_EDGE ( 'NONE', *, *, #16737, .F. ) ;
#13236 = FACE_OUTER_BOUND ( 'NONE', #12724, .T. ) ;
#13237 = AXIS2_PLACEMENT_3D ( 'NONE', #4510, #10949, #14900 ) ;
#13238 = FACE_OUTER_BOUND ( 'NONE', #7734, .T. ) ;
#13239 = DIRECTION ( 'NONE',  ( 1.000000000000000000, 0.000000000000000000, 0.000000000000000000 ) ) ;
#13240 = ORIENTED_EDGE ( 'NONE', *, *, #5204, .T. ) ;
#13241 = SURFACE_STYLE_FILL_AREA ( #14705 ) ;
#13242 = ORIENTED_EDGE ( 'NONE', *, *, #6410, .F. ) ;
#13243 = APPLICATION_CONTEXT ( 'automotive_design' ) ;
#13244 = VERTEX_POINT ( 'NONE', #16279 ) ;
#13245 = AXIS2_PLACEMENT_3D ( 'NONE', #8218, #12183, #11830 ) ;
#13246 = FACE_OUTER_BOUND ( 'NONE', #1918, .T. ) ;
#13247 = EDGE_LOOP ( 'NONE', ( #14144, #5302, #8380, #10405 ) ) ;
#13248 = SHAPE_DEFINITION_REPRESENTATION ( #12872, #12962 ) ;
#13249 = VECTOR ( 'NONE', #570, 1000.000000000000000 ) ;
#13250 = CIRCLE ( 'NONE', #12422, 8.000000000000000000 ) ;
#13251 = VERTEX_POINT ( 'NONE', #3307 ) ;
#13252 = ORIENTED_EDGE ( 'NONE', *, *, #15287, .T. ) ;
#13253 = AXIS2_PLACEMENT_3D ( 'NONE', #6151, #12601, #845 ) ;
#13254 = PLANE ( 'NONE',  #4704 ) ;
#13255 = CARTESIAN_POINT ( 'NONE',  ( -26.00000000000000000, 11.00000000000000000, -40.00000000000000711 ) ) ;
#13256 = AXIS2_PLACEMENT_3D ( 'NONE', #9303, #13089, #11787 ) ;
#13257 = VERTEX_POINT ( 'NONE', #4517 ) ;
#13258 = LINE ( 'NONE', #16763, #15177 ) ;
#13259 = CARTESIAN_POINT ( 'NONE',  ( 46.99999999999988631, 559.9933750504617365, -546.7230258972048205 ) ) ;
#13260 = ORIENTED_EDGE ( 'NONE', *, *, #5156, .T. ) ;
#13261 = AXIS2_PLACEMENT_3D ( 'NONE', #7510, #9544, #5978 ) ;
#13262 = VECTOR ( 'NONE', #9658, 1000.000000000000000 ) ;
#13263 = DIRECTION ( 'NONE',  ( 1.000000000000000000, 0.000000000000000000, 1.156482317317870344E-15 ) ) ;
#13264 = AXIS2_PLACEMENT_3D ( 'NONE', #16950, #11807, #8907 ) ;
#13265 = ORIENTED_EDGE ( 'NONE', *, *, #16722, .T. ) ;
#13266 = CARTESIAN_POINT ( 'NONE',  ( 25.99999999999999645, 0.000000000000000000, -39.99999999999999289 ) ) ;
#13267 = DIRECTION ( 'NONE',  ( 0.000000000000000000, -0.000000000000000000, 1.000000000000000000 ) ) ;
#13268 = ORIENTED_EDGE ( 'NONE', *, *, #2367, .F. ) ;
#13269 = EDGE_CURVE ( 'NONE', #14463, #7690, #16734, .T. ) ;
#13270 = DIRECTION ( 'NONE',  ( 1.000000000000000000, -0.000000000000000000, -0.000000000000000000 ) ) ;
#13271 = ORIENTED_EDGE ( 'NONE', *, *, #15504, .T. ) ;
#13272 =( LENGTH_UNIT ( ) NAMED_UNIT ( * ) SI_UNIT ( .MILLI., .METRE. ) );
#13273 = DIRECTION ( 'NONE',  ( 1.000000000000000000, -0.000000000000000000, 0.000000000000000000 ) ) ;
#13274 = VERTEX_POINT ( 'NONE', #4430 ) ;
#13275 = AXIS2_PLACEMENT_3D ( 'NONE', #3796, #2492, #10486 ) ;
#13276 = ADVANCED_FACE ( 'NONE', ( #4594 ), #5713, .F. ) ;
#13277 = EDGE_LOOP ( 'NONE', ( #15853, #9395, #11267, #7133 ) ) ;
#13279 = DIRECTION ( 'NONE',  ( 0.000000000000000000, -0.9161352426163912321, 0.4008693268837190127 ) ) ;
#13278 = VECTOR ( 'NONE', #6736, 1000.000000000000000 ) ;
#13280 = VECTOR ( 'NONE', #7934, 1000.000000000000000 ) ;
#13281 = DIRECTION ( 'NONE',  ( -0.000000000000000000, 1.000000000000000000, 7.137148015447440312E-15 ) ) ;
#13282 = LINE ( 'NONE', #227, #8885 ) ;
#13283 = ORIENTED_EDGE ( 'NONE', *, *, #6982, .T. ) ;
#13284 = DIRECTION ( 'NONE',  ( 0.000000000000000000, 0.000000000000000000, 1.000000000000000000 ) ) ;
#13285 = AXIS2_PLACEMENT_3D ( 'NONE', #8822, #5029, #1172 ) ;
#13286 = DIRECTION ( 'NONE',  ( -0.000000000000000000, -1.000000000000000000, -0.000000000000000000 ) ) ;
#13287 = CIRCLE ( 'NONE', #11628, 9.000000000000007105 ) ;
#13288 = LINE ( 'NONE', #10876, #9864 ) ;
#13289 = CARTESIAN_POINT ( 'NONE',  ( 0.000000000000000000, 341.0487089519837696, -96.50000000000331113 ) ) ;
#13290 = CARTESIAN_POINT ( 'NONE',  ( 22.99999999999998224, 10.00000000000000000, -31.99999999999998579 ) ) ;
#13291 = STYLED_ITEM ( 'NONE', ( #3273 ), #3164 ) ;
#13292 =( GEOMETRIC_REPRESENTATION_CONTEXT ( 3 ) GLOBAL_UNCERTAINTY_ASSIGNED_CONTEXT ( ( #8815 ) ) GLOBAL_UNIT_ASSIGNED_CONTEXT ( ( #13272, #14640, #5521 ) ) REPRESENTATION_CONTEXT ( 'NONE', 'WORKASPACE' ) );
#13293 = EDGE_CURVE ( 'NONE', #10521, #4853, #11527, .T. ) ;
#13294 = FACE_OUTER_BOUND ( 'NONE', #14858, .T. ) ;
#13295 = AXIS2_PLACEMENT_3D ( 'NONE', #5161, #10413, #15646 ) ;
#13297 = ORIENTED_EDGE ( 'NONE', *, *, #11904, .F. ) ;
#13296 = ORIENTED_EDGE ( 'NONE', *, *, #7925, .F. ) ;
#13298 = CARTESIAN_POINT ( 'NONE',  ( 17.00000000000000711, 355.3192028797624857, -37.21049682360899169 ) ) ;
#13299 = EDGE_CURVE ( 'NONE', #8217, #9647, #12408, .T. ) ;
#13300 = ADVANCED_FACE ( 'NONE', ( #5880 ), #16520, .T. ) ;
#13301 = EDGE_CURVE ( 'NONE', #9122, #6264, #15063, .T. ) ;
#13302 = CARTESIAN_POINT ( 'NONE',  ( 0.1218274893871210962, 285.8025109750047932, 37.43226525377778557 ) ) ;
#13303 = EDGE_CURVE ( 'NONE', #15562, #12146, #3917, .T. ) ;
#13304 = DIRECTION ( 'NONE',  ( 0.000000000000000000, 0.000000000000000000, -1.000000000000000000 ) ) ;
#13305 = DIRECTION ( 'NONE',  ( -0.000000000000000000, -1.000000000000000000, 0.000000000000000000 ) ) ;
#13306 = VERTEX_POINT ( 'NONE', #3153 ) ;
#13307 =( GEOMETRIC_REPRESENTATION_CONTEXT ( 3 ) GLOBAL_UNCERTAINTY_ASSIGNED_CONTEXT ( ( #12771 ) ) GLOBAL_UNIT_ASSIGNED_CONTEXT ( ( #4230, #1568, #1735 ) ) REPRESENTATION_CONTEXT ( 'NONE', 'WORKASPACE' ) );
#13308 = VECTOR ( 'NONE', #2029, 1000.000000000000000 ) ;
#13309 = CARTESIAN_POINT ( 'NONE',  ( 45.00000000000000000, 549.5810598491749488, -575.3306267969850296 ) ) ;
#13310 = DIRECTION ( 'NONE',  ( 0.000000000000000000, 0.000000000000000000, 1.000000000000000000 ) ) ;
#13311 = ORIENTED_EDGE ( 'NONE', *, *, #5311, .T. ) ;
#13312 = CARTESIAN_POINT ( 'NONE',  ( 31.81980515339464333, 11.00000000000000000, -31.81980515339463622 ) ) ;
#13313 = AXIS2_PLACEMENT_3D ( 'NONE', #88, #12105, #12197 ) ;
#13314 = AXIS2_PLACEMENT_3D ( 'NONE', #7020, #5819, #15018 ) ;
#13315 = CARTESIAN_POINT ( 'NONE',  ( 54.99999999999999289, 515.4878487013597805, -631.7230258972047068 ) ) ;
#13316 = CARTESIAN_POINT ( 'NONE',  ( 5.044974746830580337, 0.000000000000000000, -14.76997474683059153 ) ) ;
#13317 =( LENGTH_UNIT ( ) NAMED_UNIT ( * ) SI_UNIT ( .MILLI., .METRE. ) );
#13318 = FACE_OUTER_BOUND ( 'NONE', #12285, .T. ) ;
#13319 = ORIENTED_EDGE ( 'NONE', *, *, #9472, .F. ) ;
#13320 = DIRECTION ( 'NONE',  ( -1.000000000000000000, -0.000000000000000000, -0.000000000000000000 ) ) ;
#13321 = DIRECTION ( 'NONE',  ( -0.000000000000000000, -1.000000000000000000, -0.000000000000000000 ) ) ;
#13322 = ADVANCED_FACE ( 'NONE', ( #8389 ), #567, .T. ) ;
#13323 = DIRECTION ( 'NONE',  ( -1.000000000000000000, -0.000000000000000000, -0.000000000000000000 ) ) ;
#13324 = VECTOR ( 'NONE', #16714, 1000.000000000000000 ) ;
#13325 = EDGE_CURVE ( 'NONE', #2083, #6942, #983, .T. ) ;
#13326 = FACE_OUTER_BOUND ( 'NONE', #8264, .T. ) ;
#13327 = ORIENTED_EDGE ( 'NONE', *, *, #6592, .F. ) ;
#13328 = DIRECTION ( 'NONE',  ( -0.000000000000000000, -1.000000000000000000, 0.000000000000000000 ) ) ;
#13329 = CARTESIAN_POINT ( 'NONE',  ( 449.9999999999998295, 106.2500000000000142, 0.000000000000000000 ) ) ;
#13330 = DIRECTION ( 'NONE',  ( 0.000000000000000000, 1.000000000000000000, 0.000000000000000000 ) ) ;
#13331 = VERTEX_POINT ( 'NONE', #2258 ) ;
#13332 = FACE_OUTER_BOUND ( 'NONE', #10020, .T. ) ;
#13333 = DIRECTION ( 'NONE',  ( 0.000000000000000000, 0.000000000000000000, 1.000000000000000000 ) ) ;
#13334 = PLANE ( 'NONE',  #458 ) ;
#13335 = ORIENTED_EDGE ( 'NONE', *, *, #2269, .T. ) ;
#13336 = VECTOR ( 'NONE', #1589, 1000.000000000000000 ) ;
#13337 = CARTESIAN_POINT ( 'NONE',  ( 10.00000000000000000, 309.2289037985890445, -150.1198051533984597 ) ) ;
#13338 = EDGE_LOOP ( 'NONE', ( #1153, #5014, #13181, #2747 ) ) ;
#13339 = EDGE_LOOP ( 'NONE', ( #13518, #6835, #10928, #9020 ) ) ;
#13340 = DIRECTION ( 'NONE',  ( -0.9740972002433518906, -0.2261297071993489949, -2.769290221138109488E-17 ) ) ;
#13341 = ORIENTED_EDGE ( 'NONE', *, *, #2367, .T. ) ;
#13342 = APPLICATION_PROTOCOL_DEFINITION ( 'draft international standard', 'automotive_design', 1998, #11802 ) ;
#13343 = ORIENTED_EDGE ( 'NONE', *, *, #9601, .F. ) ;
#13344 = VECTOR ( 'NONE', #11418, 1000.000000000000000 ) ;
#13345 = ORIENTED_EDGE ( 'NONE', *, *, #13389, .T. ) ;
#13346 = AXIS2_PLACEMENT_3D ( 'NONE', #9800, #1967, #6074 ) ;
#13347 = FACE_OUTER_BOUND ( 'NONE', #6673, .T. ) ;
#13348 = CARTESIAN_POINT ( 'NONE',  ( 0.000000000000000000, 38.00000000000000711, -5.741599279633704455E-16 ) ) ;
#13349 = ORIENTED_EDGE ( 'NONE', *, *, #7804, .T. ) ;
#13350 = LINE ( 'NONE', #4240, #6938 ) ;
#13351 = PLANE ( 'NONE',  #8710 ) ;
#13352 = ORIENTED_EDGE ( 'NONE', *, *, #8448, .T. ) ;
#13353 = FACE_OUTER_BOUND ( 'NONE', #14956, .T. ) ;
#13354 = EDGE_LOOP ( 'NONE', ( #1070, #8196, #2411, #853 ) ) ;
#13355 = DIRECTION ( 'NONE',  ( 0.000000000000000000, 0.000000000000000000, -1.000000000000000000 ) ) ;
#13356 = DIRECTION ( 'NONE',  ( -0.000000000000000000, -1.000000000000000000, -0.000000000000000000 ) ) ;
#13357 = ORIENTED_EDGE ( 'NONE', *, *, #16426, .T. ) ;
#13358 = AXIS2_PLACEMENT_3D ( 'NONE', #1700, #13216, #2817 ) ;
#13359 = VECTOR ( 'NONE', #12308, 1000.000000000000000 ) ;
#13360 = CARTESIAN_POINT ( 'NONE',  ( 449.9999999999998295, 106.2500000000000142, 3.000000000000000000 ) ) ;
#13361 = ORIENTED_EDGE ( 'NONE', *, *, #1, .F. ) ;
#13362 = DIRECTION ( 'NONE',  ( 0.000000000000000000, 0.000000000000000000, -1.000000000000000000 ) ) ;
#13363 = ORIENTED_EDGE ( 'NONE', *, *, #9160, .T. ) ;
#13364 = ORIENTED_EDGE ( 'NONE', *, *, #7487, .T. ) ;
#13365 = SURFACE_STYLE_USAGE ( .BOTH. , #13186 ) ;
#13366 = DIRECTION ( 'NONE',  ( -1.000000000000000000, -0.000000000000000000, -0.000000000000000000 ) ) ;
#13367 = DIRECTION ( 'NONE',  ( -1.000000000000000000, -0.000000000000000000, -0.000000000000000000 ) ) ;
#13368 = AXIS2_PLACEMENT_3D ( 'NONE', #9769, #13959, #5965 ) ;
#13369 = EDGE_CURVE ( 'NONE', #2442, #8649, #7644, .T. ) ;
#13370 = AXIS2_PLACEMENT_3D ( 'NONE', #11597, #11689, #2750 ) ;
#13371 = DIRECTION ( 'NONE',  ( 0.000000000000000000, 0.000000000000000000, -1.000000000000000000 ) ) ;
#13372 = DIRECTION ( 'NONE',  ( 0.000000000000000000, 0.000000000000000000, -1.000000000000000000 ) ) ;
#13373 = CARTESIAN_POINT ( 'NONE',  ( 0.000000000000000000, 380.0000000000000000, 0.000000000000000000 ) ) ;
#13374 = LINE ( 'NONE', #6494, #12583 ) ;
#13375 = CARTESIAN_POINT ( 'NONE',  ( 1.223489862255693833E-15, 380.0000000000000000, -75.00000000000000000 ) ) ;
#13376 = DIRECTION ( 'NONE',  ( 0.000000000000000000, -0.6366988521258363232, 0.7711125544961918710 ) ) ;
#13377 = EDGE_CURVE ( 'NONE', #5045, #12123, #8887, .T. ) ;
#13378 = DIRECTION ( 'NONE',  ( 0.000000000000000000, 0.000000000000000000, 1.000000000000000000 ) ) ;
#13379 = DIRECTION ( 'NONE',  ( 0.000000000000000000, 1.000000000000000000, 0.000000000000000000 ) ) ;
#13381 = ORIENTED_EDGE ( 'NONE', *, *, #7050, .T. ) ;
#13380 = VERTEX_POINT ( 'NONE', #2345 ) ;
#13382 = TOROIDAL_SURFACE ( 'NONE', #7589, 4.695405383895982609, 9.000000000000000000 ) ;
#13383 = CARTESIAN_POINT ( 'NONE',  ( -3.270000000000000462, 289.4632308570086821, 37.52989836422091230 ) ) ;
#13384 = CARTESIAN_POINT ( 'NONE',  ( 0.7365999999999762737, 286.1765961517409664, 37.20123489369417058 ) ) ;
#13385 = CYLINDRICAL_SURFACE ( 'NONE', #14290, 15.00000000000000000 ) ;
#13386 = CARTESIAN_POINT ( 'NONE',  ( 394.0000000000001137, 339.1725919290084335, -111.4188657433597456 ) ) ;
#13387 = VERTEX_POINT ( 'NONE', #6278 ) ;
#13388 = ADVANCED_FACE ( 'NONE', ( #15497 ), #14207, .F. ) ;
#13389 = EDGE_CURVE ( 'NONE', #13923, #8117, #3735, .T. ) ;
#13390 = EDGE_CURVE ( 'NONE', #13856, #4729, #11532, .T. ) ;
#13391 = CARTESIAN_POINT ( 'NONE',  ( -46.99999999999988631, 473.6663340069158039, -548.2494070140132862 ) ) ;
#13392 = DIRECTION ( 'NONE',  ( -1.000000000000000000, 0.000000000000000000, 0.000000000000000000 ) ) ;
#13393 = ORIENTED_EDGE ( 'NONE', *, *, #15374, .T. ) ;
#13394 = FACE_OUTER_BOUND ( 'NONE', #14603, .T. ) ;
#13395 = EDGE_CURVE ( 'NONE', #1365, #3462, #16684, .T. ) ;
#13396 = CARTESIAN_POINT ( 'NONE',  ( 2.999999999999996891, 60.00000000000000711, 6.000000000000000000 ) ) ;
#13397 = DIRECTION ( 'NONE',  ( 0.000000000000000000, 0.000000000000000000, -1.000000000000000000 ) ) ;
#13398 = EDGE_CURVE ( 'NONE', #3717, #2065, #16767, .T. ) ;
#13400 = VERTEX_POINT ( 'NONE', #10170 ) ;
#13399 = EDGE_CURVE ( 'NONE', #3722, #15340, #7655, .T. ) ;
#13401 = ADVANCED_FACE ( 'NONE', ( #10008 ), #15243, .T. ) ;
#13402 = CARTESIAN_POINT ( 'NONE',  ( -46.99999999999988631, 549.5810598491746077, -522.8108303813202156 ) ) ;
#13403 = CARTESIAN_POINT ( 'NONE',  ( -18.00000000000001421, 10.00000000000000000, 37.00000000000000711 ) ) ;
#13404 = DIRECTION ( 'NONE',  ( 0.000000000000000000, 0.000000000000000000, 1.000000000000000000 ) ) ;
#13405 = ORIENTED_EDGE ( 'NONE', *, *, #9088, .F. ) ;
#13406 = DIRECTION ( 'NONE',  ( 0.000000000000000000, 0.000000000000000000, -1.000000000000000000 ) ) ;
#13407 = PLANE ( 'NONE',  #13155 ) ;
#13408 = AXIS2_PLACEMENT_3D ( 'NONE', #13666, #16151, #12538 ) ;
#13409 = DIRECTION ( 'NONE',  ( -1.000000000000000000, -0.000000000000000000, -0.000000000000000000 ) ) ;
#13410 = ORIENTED_EDGE ( 'NONE', *, *, #11941, .T. ) ;
#13411 = EDGE_CURVE ( 'NONE', #10297, #3745, #11371, .T. ) ;
#13412 = CARTESIAN_POINT ( 'NONE',  ( 394.0000000000001137, 240.7889724647196488, -104.9456657433598110 ) ) ;
#13413 = PRODUCT_DEFINITION_CONTEXT ( 'detailed design', #6417, 'design' ) ;
#13414 = DIRECTION ( 'NONE',  ( 0.000000000000000000, 0.000000000000000000, -1.000000000000000000 ) ) ;
#13415 = CARTESIAN_POINT ( 'NONE',  ( 0.000000000000000000, 34.88079231221936283, 28.80067286797032722 ) ) ;
#13416 = EDGE_LOOP ( 'NONE', ( #1331, #10922 ) ) ;
#13417 = DIRECTION ( 'NONE',  ( 0.000000000000000000, -1.000000000000000000, -7.137148015447440312E-15 ) ) ;
#13418 = EDGE_CURVE ( 'NONE', #5457, #8068, #8231, .T. ) ;
#13419 = CARTESIAN_POINT ( 'NONE',  ( 21.99999999999998224, 6.000000000000000000, -35.99999999999999289 ) ) ;
#13420 = DIRECTION ( 'NONE',  ( -1.000000000000000000, -0.000000000000000000, -0.000000000000000000 ) ) ;
#13421 = ORIENTED_EDGE ( 'NONE', *, *, #6474, .F. ) ;
#13422 = EDGE_CURVE ( 'NONE', #13093, #12214, #537, .T. ) ;
#13423 = ADVANCED_FACE ( 'NONE', ( #4564 ), #15219, .F. ) ;
#13424 = VECTOR ( 'NONE', #7329, 1000.000000000000000 ) ;
#13425 = LINE ( 'NONE', #2935, #10819 ) ;
#13426 = EDGE_LOOP ( 'NONE', ( #15052, #11184, #4336, #15422, #1051, #14358, #12271, #11188 ) ) ;
#13427 = ORIENTED_EDGE ( 'NONE', *, *, #10786, .T. ) ;
#13428 = CARTESIAN_POINT ( 'NONE',  ( 10.00000000000000000, 620.7506394335853201, -11.00000000000000000 ) ) ;
#13429 = ORIENTED_EDGE ( 'NONE', *, *, #1087, .F. ) ;
#13430 = SHAPE_DEFINITION_REPRESENTATION ( #7509, #7676 ) ;
#13431 = ORIENTED_EDGE ( 'NONE', *, *, #12966, .F. ) ;
#13432 = ORIENTED_EDGE ( 'NONE', *, *, #5536, .T. ) ;
#13433 = CARTESIAN_POINT ( 'NONE',  ( 22.99999999999995737, 3.000000000000000000, -33.99999999999998579 ) ) ;
#13434 = CARTESIAN_POINT ( 'NONE',  ( -22.99999999999999645, 0.000000000000000000, 37.00000000000002132 ) ) ;
#13435 = VERTEX_POINT ( 'NONE', #15040 ) ;
#13436 = CARTESIAN_POINT ( 'NONE',  ( -150.0000000000000284, 620.7506394335853201, -11.00000000000000000 ) ) ;
#13437 = DIRECTION ( 'NONE',  ( 0.000000000000000000, 0.9271838545667903109, -0.3746065934159049093 ) ) ;
#13438 = VERTEX_POINT ( 'NONE', #1900 ) ;
#13439 = AXIS2_PLACEMENT_3D ( 'NONE', #771, #8668, #10042 ) ;
#13440 = CARTESIAN_POINT ( 'NONE',  ( -20.99999999999999645, 19.00000000000000000, 35.00000000000001421 ) ) ;
#13441 = VERTEX_POINT ( 'NONE', #5934 ) ;
#13442 = DIRECTION ( 'NONE',  ( 1.000000000000000000, 0.000000000000000000, 0.000000000000000000 ) ) ;
#13443 = DIRECTION ( 'NONE',  ( -1.000000000000000000, 0.000000000000000000, 0.000000000000000000 ) ) ;
#13444 = ORIENTED_EDGE ( 'NONE', *, *, #7806, .F. ) ;
#13445 = DIRECTION ( 'NONE',  ( 0.000000000000000000, 0.9271838545667884235, -0.3746065934159091837 ) ) ;
#13446 = ORIENTED_EDGE ( 'NONE', *, *, #10665, .T. ) ;
#13447 = CARTESIAN_POINT ( 'NONE',  ( 31.81980515339464333, 11.00000000000000000, 31.81980515339463622 ) ) ;
#13448 = ORIENTED_EDGE ( 'NONE', *, *, #7179, .F. ) ;
#13449 = CIRCLE ( 'NONE', #2189, 4.695405383896011919 ) ;
#13450 = VERTEX_POINT ( 'NONE', #12629 ) ;
#13451 = ADVANCED_FACE ( 'NONE', ( #6007 ), #13753, .F. ) ;
#13452 = PLANE ( 'NONE',  #11822 ) ;
#13453 = DIRECTION ( 'NONE',  ( 0.000000000000000000, 1.000000000000000000, 0.000000000000000000 ) ) ;
#13454 = DIRECTION ( 'NONE',  ( -0.000000000000000000, -1.000000000000000000, 0.000000000000000000 ) ) ;
#13455 = PRODUCT ( 'Servo-Body.2', 'Servo-Body.2', '', ( #13752 ) ) ;
#13456 = CARTESIAN_POINT ( 'NONE',  ( -30.99999999999999645, 68.00000000000000000, -30.99999999999999289 ) ) ;
#13457 = EDGE_CURVE ( 'NONE', #16470, #1459, #11096, .T. ) ;
#13458 = DIRECTION ( 'NONE',  ( 0.000000000000000000, 1.000000000000000000, 0.000000000000000000 ) ) ;
#13459 = CARTESIAN_POINT ( 'NONE',  ( -40.00000000000000000, 0.000000000000000000, 26.00000000000000355 ) ) ;
#13460 = DIRECTION ( 'NONE',  ( 0.000000000000000000, 0.000000000000000000, -1.000000000000000000 ) ) ;
#13461 = CARTESIAN_POINT ( 'NONE',  ( 49.99999999999999289, 515.4878487013597805, -606.7230258972047068 ) ) ;
#13462 = AXIS2_PLACEMENT_3D ( 'NONE', #10398, #8858, #7809 ) ;
#13463 = TOROIDAL_SURFACE ( 'NONE', #9607, 4.695405383895982609, 9.000000000000000000 ) ;
#13464 = LINE ( 'NONE', #13709, #933 ) ;
#13465 = DIRECTION ( 'NONE',  ( 1.000000000000000000, 0.000000000000000000, 0.000000000000000000 ) ) ;
#13467 = ORIENTED_EDGE ( 'NONE', *, *, #10247, .T. ) ;
#13466 = ORIENTED_EDGE ( 'NONE', *, *, #8561, .T. ) ;
#13468 = CARTESIAN_POINT ( 'NONE',  ( 2.903217335657448661, 40.21902629923274475, 9.045605051663343943 ) ) ;
#13469 = PRODUCT_DEFINITION ( 'UNKNOWN', '', #9193, #8956 ) ;
#13470 = DIRECTION ( 'NONE',  ( 0.000000000000000000, -0.3420201433256630508, -0.9396926207859104263 ) ) ;
#13471 = FACE_OUTER_BOUND ( 'NONE', #1592, .T. ) ;
#13472 = PLANE ( 'NONE',  #1740 ) ;
#13473 = EDGE_CURVE ( 'NONE', #15272, #10013, #12301, .T. ) ;
#13474 = VERTEX_POINT ( 'NONE', #14968 ) ;
#13475 = DIRECTION ( 'NONE',  ( -0.000000000000000000, -0.000000000000000000, 1.000000000000000000 ) ) ;
#13476 = CARTESIAN_POINT ( 'NONE',  ( -22.99999999999999645, 68.00000000000000000, -36.99999999999999289 ) ) ;
#13477 = ORIENTED_EDGE ( 'NONE', *, *, #15763, .F. ) ;
#13478 = CARTESIAN_POINT ( 'NONE',  ( 46.99999999999988631, 493.2350855268092573, -585.2659423243250103 ) ) ;
#13479 = DIRECTION ( 'NONE',  ( -0.000000000000000000, 1.000000000000000000, -2.081668171172169499E-16 ) ) ;
#13480 = CARTESIAN_POINT ( 'NONE',  ( -49.99999999999999289, 515.4878487013597805, -546.7230258972048205 ) ) ;
#13481 = CARTESIAN_POINT ( 'NONE',  ( 0.000000000000000000, 106.2500000000000142, 3.000000000000000000 ) ) ;
#13482 = CARTESIAN_POINT ( 'NONE',  ( 39.99999999999999289, 0.000000000000000000, 26.00000000000000000 ) ) ;
#13483 = CARTESIAN_POINT ( 'NONE',  ( -13.11912225705329327, 0.000000000000000000, 22.50000000000000000 ) ) ;
#13484 = ORIENTED_EDGE ( 'NONE', *, *, #14351, .T. ) ;
#13485 = AXIS2_PLACEMENT_3D ( 'NONE', #1674, #3149, #481 ) ;
#13486 = DIRECTION ( 'NONE',  ( 0.000000000000000000, 0.8660254037844432595, -0.4999999999999919509 ) ) ;
#13487 = ADVANCED_FACE ( 'NONE', ( #16246 ), #868, .T. ) ;
#13488 = LINE ( 'NONE', #4115, #14808 ) ;
#13489 = DIRECTION ( 'NONE',  ( -0.000000000000000000, -1.000000000000000000, 0.000000000000000000 ) ) ;
#13490 = EDGE_CURVE ( 'NONE', #10460, #14475, #7213, .T. ) ;
#13491 = ORIENTED_EDGE ( 'NONE', *, *, #15185, .F. ) ;
#13492 = PLANE ( 'NONE',  #4452 ) ;
#13493 = LINE ( 'NONE', #10026, #6655 ) ;
#13494 = ORIENTED_EDGE ( 'NONE', *, *, #280, .F. ) ;
#13495 = FACE_OUTER_BOUND ( 'NONE', #6270, .T. ) ;
#13496 = DIRECTION ( 'NONE',  ( 1.156482317317870344E-15, 0.000000000000000000, -1.000000000000000000 ) ) ;
#13497 = DIRECTION ( 'NONE',  ( 0.000000000000000000, 1.000000000000000000, -1.224646799147353207E-16 ) ) ;
#13498 = VERTEX_POINT ( 'NONE', #1826 ) ;
#13499 = CIRCLE ( 'NONE', #9665, 10.00000000000061995 ) ;
#13500 = AXIS2_PLACEMENT_3D ( 'NONE', #12784, #10887, #13470 ) ;
#13501 = ORIENTED_EDGE ( 'NONE', *, *, #11783, .T. ) ;
#13502 = VERTEX_POINT ( 'NONE', #7046 ) ;
#13503 = CARTESIAN_POINT ( 'NONE',  ( 26.00000000000000000, 11.00000000000000000, 31.00000000000003197 ) ) ;
#13504 = EDGE_CURVE ( 'NONE', #8747, #8625, #10687, .T. ) ;
#13505 = ORIENTED_EDGE ( 'NONE', *, *, #12664, .F. ) ;
#13506 = AXIS2_PLACEMENT_3D ( 'NONE', #15645, #1392, #5160 ) ;
#13507 = VERTEX_POINT ( 'NONE', #11010 ) ;
#13508 = ADVANCED_FACE ( 'NONE', ( #12380 ), #3281, .F. ) ;
#13509 = EDGE_CURVE ( 'NONE', #478, #2521, #3364, .T. ) ;
#13510 = EDGE_CURVE ( 'NONE', #3270, #197, #7299, .T. ) ;
#13511 = VECTOR ( 'NONE', #3827, 1000.000000000000000 ) ;
#13512 = ORIENTED_EDGE ( 'NONE', *, *, #5470, .T. ) ;
#13513 = EDGE_CURVE ( 'NONE', #11776, #5137, #14596, .T. ) ;
#13514 = CIRCLE ( 'NONE', #2518, 10.00000000000000178 ) ;
#13515 = VECTOR ( 'NONE', #4002, 1000.000000000000000 ) ;
#13516 = LINE ( 'NONE', #8094, #4166 ) ;
#13517 = DIRECTION ( 'NONE',  ( 1.000000000000000000, 0.000000000000000000, 0.000000000000000000 ) ) ;
#13518 = ORIENTED_EDGE ( 'NONE', *, *, #14354, .F. ) ;
#13519 = LINE ( 'NONE', #13607, #2551 ) ;
#13520 = FACE_OUTER_BOUND ( 'NONE', #1288, .T. ) ;
#13521 = ORIENTED_EDGE ( 'NONE', *, *, #16048, .F. ) ;
#13522 = CIRCLE ( 'NONE', #9120, 9.999999999999998224 ) ;
#13523 = CARTESIAN_POINT ( 'NONE',  ( -3.270000000000002238, 239.4632308570078294, 71.73739990498292229 ) ) ;
#13524 = ORIENTED_EDGE ( 'NONE', *, *, #1108, .T. ) ;
#13525 = CARTESIAN_POINT ( 'NONE',  ( 0.000000000000000000, 240.7889724647196488, -104.2090657433598011 ) ) ;
#13526 = FACE_OUTER_BOUND ( 'NONE', #14810, .T. ) ;
#13527 = VERTEX_POINT ( 'NONE', #4208 ) ;
#13528 = AXIS2_PLACEMENT_3D ( 'NONE', #3432, #7437, #7278 ) ;
#13529 = EDGE_LOOP ( 'NONE', ( #11455, #16511, #10047, #9497, #7492, #6714 ) ) ;
#13530 = DIRECTION ( 'NONE',  ( 1.000000000000000000, -1.476083657435421627E-31, -7.888609052210118054E-31 ) ) ;
#13531 = DIRECTION ( 'NONE',  ( -0.000000000000000000, -0.000000000000000000, 1.000000000000000000 ) ) ;
#13532 = ORIENTED_EDGE ( 'NONE', *, *, #15050, .F. ) ;
#13533 = CIRCLE ( 'NONE', #8308, 4.999999999999990230 ) ;
#13534 = ORIENTED_EDGE ( 'NONE', *, *, #8121, .F. ) ;
#13535 = CARTESIAN_POINT ( 'NONE',  ( -45.00000000000000000, 523.2161522479893847, -576.8570079137933817 ) ) ;
#13536 = EDGE_CURVE ( 'NONE', #14008, #16924, #8066, .T. ) ;
#13537 = DIRECTION ( 'NONE',  ( -1.000000000000000000, 0.000000000000000000, -0.000000000000000000 ) ) ;
#13538 = FACE_OUTER_BOUND ( 'NONE', #7270, .T. ) ;
#13539 = AXIS2_PLACEMENT_3D ( 'NONE', #11533, #5004, #2689 ) ;
#13540 = DIRECTION ( 'NONE',  ( 0.000000000000000000, 0.000000000000000000, -1.000000000000000000 ) ) ;
#13541 = AXIS2_PLACEMENT_3D ( 'NONE', #6623, #11886, #129 ) ;
#13542 = AXIS2_PLACEMENT_3D ( 'NONE', #1692, #1789, #10627 ) ;
#13543 = DIRECTION ( 'NONE',  ( 0.000000000000000000, 0.000000000000000000, -1.000000000000000000 ) ) ;
#13544 = CARTESIAN_POINT ( 'NONE',  ( 0.2121372864226510613, 189.4665531203498858, 37.56312099760641132 ) ) ;
#13545 = PLANE ( 'NONE',  #8472 ) ;
#13546 = CARTESIAN_POINT ( 'NONE',  ( -2.216159785453297477E-13, 106.2500000000000142, 0.000000000000000000 ) ) ;
#13547 = DIRECTION ( 'NONE',  ( -0.000000000000000000, -1.000000000000000000, -0.000000000000000000 ) ) ;
#13548 = VECTOR ( 'NONE', #13684, 1000.000000000000000 ) ;
#13549 = FACE_OUTER_BOUND ( 'NONE', #13006, .T. ) ;
#13550 = DIRECTION ( 'NONE',  ( 0.000000000000000000, 0.000000000000000000, 1.000000000000000000 ) ) ;
#13552 = ORIENTED_EDGE ( 'NONE', *, *, #11673, .F. ) ;
#13551 = ORIENTED_EDGE ( 'NONE', *, *, #6211, .F. ) ;
#13553 = AXIS2_PLACEMENT_3D ( 'NONE', #9212, #12984, #3974 ) ;
#13554 = DIRECTION ( 'NONE',  ( -1.000000000000000000, 0.000000000000000000, 0.000000000000000000 ) ) ;
#13555 = VECTOR ( 'NONE', #8721, 1000.000000000000000 ) ;
#13556 = VECTOR ( 'NONE', #13367, 1000.000000000000000 ) ;
#13557 = CARTESIAN_POINT ( 'NONE',  ( 0.2120431089095113630, 289.4599079970928415, 37.56312696337874257 ) ) ;
#13558 = DIRECTION ( 'NONE',  ( 1.000000000000000000, 0.000000000000000000, -3.854941057726258312E-16 ) ) ;
#13559 = FACE_OUTER_BOUND ( 'NONE', #9653, .T. ) ;
#13560 = AXIS2_PLACEMENT_3D ( 'NONE', #3460, #16591, #7383 ) ;
#13561 = ORIENTED_EDGE ( 'NONE', *, *, #3733, .F. ) ;
#13562 = CARTESIAN_POINT ( 'NONE',  ( -270.0000000000000000, 620.7506394335853201, 0.000000000000000000 ) ) ;
#13563 =( GEOMETRIC_REPRESENTATION_CONTEXT ( 3 ) GLOBAL_UNCERTAINTY_ASSIGNED_CONTEXT ( ( #14600 ) ) GLOBAL_UNIT_ASSIGNED_CONTEXT ( ( #955, #16583, #3612 ) ) REPRESENTATION_CONTEXT ( 'NONE', 'WORKASPACE' ) );
#13564 = DIRECTION ( 'NONE',  ( 1.000000000000000000, -0.000000000000000000, -0.000000000000000000 ) ) ;
#13565 = ORIENTED_EDGE ( 'NONE', *, *, #1998, .F. ) ;
#13566 = DIRECTION ( 'NONE',  ( 0.000000000000000000, 0.000000000000000000, -1.000000000000000000 ) ) ;
#13567 = VECTOR ( 'NONE', #10070, 1000.000000000000000 ) ;
#13568 = DIRECTION ( 'NONE',  ( -0.000000000000000000, -0.000000000000000000, 1.000000000000000000 ) ) ;
#13569 = CARTESIAN_POINT ( 'NONE',  ( 25.99999999999997868, 10.00000000000000000, -39.99999999999999289 ) ) ;
#13570 = CIRCLE ( 'NONE', #11355, 4.999999999999997335 ) ;
#13571 = DIRECTION ( 'NONE',  ( 0.000000000000000000, 1.000000000000000000, 0.000000000000000000 ) ) ;
#13572 = ORIENTED_EDGE ( 'NONE', *, *, #1292, .T. ) ;
#13573 = LINE ( 'NONE', #10987, #11929 ) ;
#13574 = AXIS2_PLACEMENT_3D ( 'NONE', #7821, #11777, #8955 ) ;
#13575 = CARTESIAN_POINT ( 'NONE',  ( -22.00000000000001776, 8.000000000000000000, 36.00000000000000711 ) ) ;
#13576 = APPLICATION_CONTEXT ( 'automotive_design' ) ;
#13577 = FILL_AREA_STYLE_COLOUR ( '', #10226 ) ;
#13578 = VERTEX_POINT ( 'NONE', #15875 ) ;
#13579 = AXIS2_PLACEMENT_3D ( 'NONE', #9468, #10837, #1823 ) ;
#13580 = CARTESIAN_POINT ( 'NONE',  ( 5.941205806953520074, 1.854262922671694143E-15, 15.14120580695351670 ) ) ;
#13581 = PRODUCT_DEFINITION_CONTEXT ( 'detailed design', #11474, 'design' ) ;
#13582 = EDGE_CURVE ( 'NONE', #882, #12485, #4303, .T. ) ;
#13583 = CYLINDRICAL_SURFACE ( 'NONE', #9222, 13.69540538389601991 ) ;
#13584 = ORIENTED_EDGE ( 'NONE', *, *, #7989, .T. ) ;
#13585 = CARTESIAN_POINT ( 'NONE',  ( 39.06972645625037899, 346.7108172824755457, -6.736600000000000144 ) ) ;
#13586 = CARTESIAN_POINT ( 'NONE',  ( 10.00000000000000000, 435.2933666400819561, -550.3792044179907634 ) ) ;
#13587 = DIRECTION ( 'NONE',  ( 0.000000000000000000, -1.000000000000000000, -1.321694076934710402E-16 ) ) ;
#13588 = ORIENTED_EDGE ( 'NONE', *, *, #4264, .F. ) ;
#13589 = CARTESIAN_POINT ( 'NONE',  ( 23.00000000000000711, 0.000000000000000000, -31.00000000000002487 ) ) ;
#13590 =( NAMED_UNIT ( * ) PLANE_ANGLE_UNIT ( ) SI_UNIT ( $, .RADIAN. ) );
#13591 = EDGE_LOOP ( 'NONE', ( #908, #11899, #6682, #9035 ) ) ;
#13592 = ORIENTED_EDGE ( 'NONE', *, *, #13162, .F. ) ;
#13593 = EDGE_CURVE ( 'NONE', #9116, #4106, #2827, .T. ) ;
#13594 = DIRECTION ( 'NONE',  ( -0.000000000000000000, -0.000000000000000000, 1.000000000000000000 ) ) ;
#13595 = CIRCLE ( 'NONE', #8916, 12.50000000000001066 ) ;
#13596 = ORIENTED_EDGE ( 'NONE', *, *, #5379, .T. ) ;
#13597 = DIRECTION ( 'NONE',  ( 0.000000000000000000, 0.000000000000000000, 1.000000000000000000 ) ) ;
#13598 = PRODUCT_DEFINITION_SHAPE ( 'NONE', 'NONE',  #10624 ) ;
#13599 = VERTEX_POINT ( 'NONE', #1804 ) ;
#13600 = CARTESIAN_POINT ( 'NONE',  ( 2.600106608147765286, 61.50910620841189314, 9.137947797636652325 ) ) ;
#13601 = EDGE_LOOP ( 'NONE', ( #12279, #8700, #3250, #2680 ) ) ;
#13602 = DIRECTION ( 'NONE',  ( -0.000000000000000000, 0.000000000000000000, -1.000000000000000000 ) ) ;
#13603 = DIRECTION ( 'NONE',  ( 1.000000000000000000, 0.000000000000000000, 0.000000000000000000 ) ) ;
#13604 = EDGE_CURVE ( 'NONE', #12123, #9647, #13488, .T. ) ;
#13605 = EDGE_LOOP ( 'NONE', ( #7761, #11857 ) ) ;
#13606 = VECTOR ( 'NONE', #15582, 1000.000000000000000 ) ;
#13607 = CARTESIAN_POINT ( 'NONE',  ( 21.00000000000000000, 8.000000000000000000, -31.00000000000003908 ) ) ;
#13608 = CARTESIAN_POINT ( 'NONE',  ( -18.00000000000001421, 6.000000000000000000, 40.00000000000000711 ) ) ;
#13609 = ORIENTED_EDGE ( 'NONE', *, *, #143, .F. ) ;
#13610 = DIRECTION ( 'NONE',  ( 4.930380657631322689E-32, 0.09950371902099953980, 0.9950371902099890420 ) ) ;
#13611 = PRODUCT_DEFINITION_SHAPE ( 'NONE', 'NONE',  #1808 ) ;
#13612 = EDGE_CURVE ( 'NONE', #9012, #5898, #4915, .T. ) ;
#13613 = ORIENTED_EDGE ( 'NONE', *, *, #189, .T. ) ;
#13614 = CARTESIAN_POINT ( 'NONE',  ( 45.00000000000000000, 523.2161522479888163, -489.1982331128240276 ) ) ;
#13615 = EDGE_LOOP ( 'NONE', ( #8131, #3889, #1801, #4398 ) ) ;
#13616 = EDGE_CURVE ( 'NONE', #15821, #452, #2174, .T. ) ;
#13617 = EDGE_CURVE ( 'NONE', #1326, #9930, #15613, .T. ) ;
#13618 = ORIENTED_EDGE ( 'NONE', *, *, #15050, .T. ) ;
#13619 = FACE_OUTER_BOUND ( 'NONE', #6480, .T. ) ;
#13620 = VECTOR ( 'NONE', #12065, 1000.000000000000000 ) ;
#13621 = ORIENTED_EDGE ( 'NONE', *, *, #8464, .F. ) ;
#13622 = VERTEX_POINT ( 'NONE', #435 ) ;
#13623 = DIRECTION ( 'NONE',  ( 0.000000000000000000, 0.000000000000000000, 1.000000000000000000 ) ) ;
#13624 = FACE_OUTER_BOUND ( 'NONE', #14021, .T. ) ;
#13625 = CARTESIAN_POINT ( 'NONE',  ( 0.7365999999999927050, 189.4632308570089094, 37.52989836422091940 ) ) ;
#13626 = DIRECTION ( 'NONE',  ( -0.000000000000000000, -0.000000000000000000, 1.000000000000000000 ) ) ;
#13627 = CARTESIAN_POINT ( 'NONE',  ( -21.00000000000002842, -20.00000000000000000, -34.99999999999999289 ) ) ;
#13628 = AXIS2_PLACEMENT_3D ( 'NONE', #12597, #11308, #3501 ) ;
#13629 = CARTESIAN_POINT ( 'NONE',  ( 35.99999999999999289, 6.000000000000000000, 21.99999999999999645 ) ) ;
#13630 = AXIS2_PLACEMENT_3D ( 'NONE', #1356, #15362, #8837 ) ;
#13631 = FACE_OUTER_BOUND ( 'NONE', #5985, .T. ) ;
#13632 = ADVANCED_FACE ( 'NONE', ( #10909 ), #8325, .T. ) ;
#13633 = LINE ( 'NONE', #822, #12533 ) ;
#13634 = CARTESIAN_POINT ( 'NONE',  ( -25.99999999999999645, 68.00000000000000000, 40.00000000000002132 ) ) ;
#13635 = EDGE_CURVE ( 'NONE', #14813, #2243, #1628, .T. ) ;
#13636 = EDGE_CURVE ( 'NONE', #12302, #997, #15080, .T. ) ;
#13637 = CARTESIAN_POINT ( 'NONE',  ( 30.99999999999999645, 0.000000000000000000, 26.00000000000001066 ) ) ;
#13638 = CARTESIAN_POINT ( 'NONE',  ( 31.00000000000003553, 19.00000000000000000, 25.99999999999999645 ) ) ;
#13640 = ORIENTED_EDGE ( 'NONE', *, *, #14983, .T. ) ;
#13639 = ORIENTED_EDGE ( 'NONE', *, *, #5379, .F. ) ;
#13641 = CARTESIAN_POINT ( 'NONE',  ( 0.000000000000000000, 341.5974953295075807, -105.4170192159777031 ) ) ;
#13642 = VECTOR ( 'NONE', #13568, 1000.000000000000000 ) ;
#13643 = VECTOR ( 'NONE', #11971, 1000.000000000000000 ) ;
#13644 = DIRECTION ( 'NONE',  ( -0.000000000000000000, -0.000000000000000000, -1.000000000000000000 ) ) ;
#13645 = LINE ( 'NONE', #12343, #14906 ) ;
#13646 = ORIENTED_EDGE ( 'NONE', *, *, #1128, .T. ) ;
#13647 = FACE_BOUND ( 'NONE', #3940, .T. ) ;
#13648 = ORIENTED_EDGE ( 'NONE', *, *, #2049, .F. ) ;
#13649 = PLANE ( 'NONE',  #7943 ) ;
#13650 = CARTESIAN_POINT ( 'NONE',  ( -3.197567832863594806, 192.4311383381408689, 37.56865621330425853 ) ) ;
#13651 = DIRECTION ( 'NONE',  ( -0.000000000000000000, -1.000000000000000000, -0.000000000000000000 ) ) ;
#13652 = AXIS2_PLACEMENT_3D ( 'NONE', #7493, #4922, #1065 ) ;
#13653 = PLANE ( 'NONE',  #4799 ) ;
#13654 = SURFACE_STYLE_FILL_AREA ( #8413 ) ;
#13655 = EDGE_LOOP ( 'NONE', ( #9697, #5574 ) ) ;
#13656 = DIRECTION ( 'NONE',  ( 1.000000000000000000, -0.000000000000000000, 0.000000000000000000 ) ) ;
#13657 = LINE ( 'NONE', #7434, #9872 ) ;
#13658 = DIRECTION ( 'NONE',  ( 0.000000000000000000, -1.000000000000000000, 0.000000000000000000 ) ) ;
#13659 = AXIS2_PLACEMENT_3D ( 'NONE', #3858, #2395, #16900 ) ;
#13660 = VERTEX_POINT ( 'NONE', #6939 ) ;
#13661 = EDGE_CURVE ( 'NONE', #3874, #2075, #4457, .T. ) ;
#13662 = LINE ( 'NONE', #604, #5827 ) ;
#13663 = LINE ( 'NONE', #1887, #2366 ) ;
#13664 = VERTEX_POINT ( 'NONE', #12198 ) ;
#13665 = CARTESIAN_POINT ( 'NONE',  ( -5.000000000000000888, 0.000000000000000000, 0.000000000000000000 ) ) ;
#13666 = CARTESIAN_POINT ( 'NONE',  ( 1.224999999999999867, 0.000000000000000000, 0.000000000000000000 ) ) ;
#13667 = DIRECTION ( 'NONE',  ( -1.000000000000000000, -0.000000000000000000, -0.000000000000000000 ) ) ;
#13668 = ORIENTED_EDGE ( 'NONE', *, *, #16229, .F. ) ;
#13669 = ADVANCED_FACE ( 'NONE', ( #7969 ), #4385, .F. ) ;
#13670 = CARTESIAN_POINT ( 'NONE',  ( -31.81980515339462912, 11.00000000000000000, -31.81980515339465043 ) ) ;
#13671 = EDGE_LOOP ( 'NONE', ( #13688, #11009, #165, #16802 ) ) ;
#13672 = ORIENTED_EDGE ( 'NONE', *, *, #3427, .F. ) ;
#13673 = CARTESIAN_POINT ( 'NONE',  ( 23.00000000000001066, 68.00000000000000000, -36.99999999999999289 ) ) ;
#13674 = TOROIDAL_SURFACE ( 'NONE', #12572, 4.695405383895982609, 9.000000000000000000 ) ;
#13675 = SHAPE_DEFINITION_REPRESENTATION ( #3828, #11211 ) ;
#13676 = PRODUCT_RELATED_PRODUCT_CATEGORY ( 'part', '', ( #13455 ) ) ;
#13677 = EDGE_LOOP ( 'NONE', ( #2180, #13427, #16011, #12566 ) ) ;
#13678 = CARTESIAN_POINT ( 'NONE',  ( 2.844582250340499385, 60.97290968073905759, 9.064464814046607088 ) ) ;
#13679 = ORIENTED_EDGE ( 'NONE', *, *, #12461, .T. ) ;
#13680 = CARTESIAN_POINT ( 'NONE',  ( 35.00000000000003553, -20.00000000000000000, -20.99999999999999645 ) ) ;
#13681 = FACE_OUTER_BOUND ( 'NONE', #7442, .T. ) ;
#13682 = EDGE_CURVE ( 'NONE', #14008, #13213, #9709, .T. ) ;
#13683 = ORIENTED_EDGE ( 'NONE', *, *, #8882, .T. ) ;
#13684 = DIRECTION ( 'NONE',  ( -0.000000000000000000, -0.000000000000000000, 1.000000000000000000 ) ) ;
#13685 = VECTOR ( 'NONE', #527, 1000.000000000000000 ) ;
#13686 = DIRECTION ( 'NONE',  ( -1.000000000000000000, -0.000000000000000000, -0.000000000000000000 ) ) ;
#13687 = ORIENTED_EDGE ( 'NONE', *, *, #3756, .F. ) ;
#13688 = ORIENTED_EDGE ( 'NONE', *, *, #15234, .F. ) ;
#13689 = CARTESIAN_POINT ( 'NONE',  ( 1.224646799147349016E-16, 66.00000000000000000, -0.9999999999999972244 ) ) ;
#13690 = EDGE_LOOP ( 'NONE', ( #6584, #3315, #10489, #8807 ) ) ;
#13691 = ORIENTED_EDGE ( 'NONE', *, *, #11517, .T. ) ;
#13692 = ADVANCED_FACE ( 'NONE', ( #5397 ), #12022, .F. ) ;
#13693 = VERTEX_POINT ( 'NONE', #2920 ) ;
#13694 =( REPRESENTATION_RELATIONSHIP ('NONE','NONE', #15277, #2419 ) REPRESENTATION_RELATIONSHIP_WITH_TRANSFORMATION ( #6175 )SHAPE_REPRESENTATION_RELATIONSHIP( ) );
#13695 = ORIENTED_EDGE ( 'NONE', *, *, #598, .F. ) ;
#13696 = FACE_OUTER_BOUND ( 'NONE', #4880, .T. ) ;
#13697 = LINE ( 'NONE', #12573, #861 ) ;
#13698 = CARTESIAN_POINT ( 'NONE',  ( 45.00000000000000000, 515.4878487013597805, -546.7230258972048205 ) ) ;
#13699 = ADVANCED_FACE ( 'NONE', ( #8159 ), #13407, .T. ) ;
#13700 = ADVANCED_FACE ( 'NONE', ( #16057 ), #13714, .F. ) ;
#13701 = VECTOR ( 'NONE', #9414, 1000.000000000000000 ) ;
#13702 = CARTESIAN_POINT ( 'NONE',  ( -0.9999999999999991118, 2.755455298081544778E-15, -22.50000000000000000 ) ) ;
#13703 = CARTESIAN_POINT ( 'NONE',  ( 34.00000000000002842, 0.000000000000000000, 31.00000000000000000 ) ) ;
#13704 = DIRECTION ( 'NONE',  ( 0.000000000000000000, 0.000000000000000000, 1.000000000000000000 ) ) ;
#13705 = DIRECTION ( 'NONE',  ( -0.000000000000000000, -1.000000000000000000, -0.000000000000000000 ) ) ;
#13706 = ORIENTED_EDGE ( 'NONE', *, *, #13593, .F. ) ;
#13707 = DIRECTION ( 'NONE',  ( -1.000000000000000000, 0.000000000000000000, 0.000000000000000000 ) ) ;
#13708 = DIRECTION ( 'NONE',  ( -0.000000000000000000, 0.7625786632508375629, 0.6468954956981580739 ) ) ;
#13709 = CARTESIAN_POINT ( 'NONE',  ( 36.99999999999999289, 6.000000000000000000, 22.99999999999999645 ) ) ;
#13710 = CARTESIAN_POINT ( 'NONE',  ( 31.00000000000000000, 19.00000000000000000, -21.00000000000000355 ) ) ;
#13712 = ORIENTED_EDGE ( 'NONE', *, *, #16542, .T. ) ;
#13711 = ORIENTED_EDGE ( 'NONE', *, *, #15070, .F. ) ;
#13713 = DIRECTION ( 'NONE',  ( 0.000000000000000000, 0.000000000000000000, -1.000000000000000000 ) ) ;
#13714 = CONICAL_SURFACE ( 'NONE', #3290, 13.62500000000000000, 0.2281026282799422378 ) ;
#13715 = EDGE_CURVE ( 'NONE', #15604, #4249, #935, .T. ) ;
#13716 = SURFACE_STYLE_FILL_AREA ( #4606 ) ;
#13717 = CARTESIAN_POINT ( 'NONE',  ( -55.99999999999988631, 645.2345343053611941, -411.3640676610526157 ) ) ;
#13718 = EDGE_CURVE ( 'NONE', #3738, #1429, #13657, .T. ) ;
#13719 = LINE ( 'NONE', #8564, #646 ) ;
#13720 = EDGE_CURVE ( 'NONE', #11801, #7178, #3508, .T. ) ;
#13722 = ORIENTED_EDGE ( 'NONE', *, *, #10007, .T. ) ;
#13721 = EDGE_CURVE ( 'NONE', #16479, #6189, #4620, .T. ) ;
#13723 = EDGE_CURVE ( 'NONE', #2662, #1311, #5176, .T. ) ;
#13724 = VECTOR ( 'NONE', #9773, 1000.000000000000000 ) ;
#13725 = CARTESIAN_POINT ( 'NONE',  ( 0.000000000000000000, 380.0000000000000000, 0.000000000000000000 ) ) ;
#13726 = VERTEX_POINT ( 'NONE', #2209 ) ;
#13727 = CARTESIAN_POINT ( 'NONE',  ( -45.00000000000000000, 523.2161522479888163, -502.8936384967199729 ) ) ;
#13728 = AXIS2_PLACEMENT_3D ( 'NONE', #7096, #5814, #11060 ) ;
#13729 = CARTESIAN_POINT ( 'NONE',  ( -3.165718926336553274, 192.4396550164971700, 37.56780454546862558 ) ) ;
#13730 = DIRECTION ( 'NONE',  ( 1.000000000000000000, 0.000000000000000000, -0.000000000000000000 ) ) ;
#13731 = PRODUCT_DEFINITION_SHAPE ( 'NONE', 'NONE',  #16986 ) ;
#13732 = PLANE ( 'NONE',  #2514 ) ;
#13733 = FACE_OUTER_BOUND ( 'NONE', #16198, .T. ) ;
#13734 = ORIENTED_EDGE ( 'NONE', *, *, #5705, .F. ) ;
#13735 = CARTESIAN_POINT ( 'NONE',  ( -8.881784197001250351E-16, 0.000000000000000000, 0.000000000000000000 ) ) ;
#13736 = AXIS2_PLACEMENT_3D ( 'NONE', #10601, #4077, #8011 ) ;
#13737 = DIRECTION ( 'NONE',  ( 0.000000000000000000, 0.000000000000000000, -1.000000000000000000 ) ) ;
#13738 = ORIENTED_EDGE ( 'NONE', *, *, #15988, .T. ) ;
#13739 = EDGE_CURVE ( 'NONE', #3294, #4443, #6067, .T. ) ;
#13740 = PLANE ( 'NONE',  #909 ) ;
#13741 = CARTESIAN_POINT ( 'NONE',  ( 0.000000000000000000, 435.2933666400819561, -550.3792044179907634 ) ) ;
#13742 = VERTEX_POINT ( 'NONE', #11408 ) ;
#13743 = DIRECTION ( 'NONE',  ( 0.000000000000000000, 0.000000000000000000, 1.000000000000000000 ) ) ;
#13744 = CARTESIAN_POINT ( 'NONE',  ( -35.00000000000000000, 8.000000000000000000, 20.99999999999999289 ) ) ;
#13745 = DIRECTION ( 'NONE',  ( 0.000000000000000000, 1.000000000000000000, 0.000000000000000000 ) ) ;
#13746 = ORIENTED_EDGE ( 'NONE', *, *, #12341, .T. ) ;
#13747 = AXIS2_PLACEMENT_3D ( 'NONE', #9339, #958, #6176 ) ;
#13748 = ORIENTED_EDGE ( 'NONE', *, *, #8020, .T. ) ;
#13749 = ORIENTED_EDGE ( 'NONE', *, *, #8964, .F. ) ;
#13750 = DIRECTION ( 'NONE',  ( 0.000000000000000000, 1.000000000000000000, 0.000000000000000000 ) ) ;
#13751 = EDGE_CURVE ( 'NONE', #4924, #1561, #4387, .T. ) ;
#13752 = PRODUCT_CONTEXT ( 'NONE', #306, 'mechanical' ) ;
#13753 = PLANE ( 'NONE',  #12337 ) ;
#13754 = AXIS2_PLACEMENT_3D ( 'NONE', #2785, #11805, #6294 ) ;
#13755 = ORIENTED_EDGE ( 'NONE', *, *, #8559, .F. ) ;
#13756 = CARTESIAN_POINT ( 'NONE',  ( 65.00000000000000000, 380.0000000000000000, -7.000000000000006217 ) ) ;
#13757 = CARTESIAN_POINT ( 'NONE',  ( 394.0000000000001137, 339.1725919290087745, -10.68226574335978718 ) ) ;
#13758 = ORIENTED_EDGE ( 'NONE', *, *, #69, .T. ) ;
#13759 = DIRECTION ( 'NONE',  ( 1.156482317317881191E-15, 0.000000000000000000, 1.000000000000000000 ) ) ;
#13760 = CLOSED_SHELL ( 'NONE', ( #9712, #5936, #8824, #1354, #5065, #1738, #14568, #10927, #3820, #13965, #8981, #15886, #2771, #9676, #3539, #16933, #11077, #12031, #2994, #7511, #10410, #8770, #15706, #15573, #12611, #6311, #9005, #7087 ) ) ;
#13761 = COLOUR_RGB ( '', 0.09019608, 0.27058824, 0.51372549) ;
#13762 = DIRECTION ( 'NONE',  ( 0.000000000000000000, 1.000000000000000000, 0.000000000000000000 ) ) ;
#13763 = ORIENTED_EDGE ( 'NONE', *, *, #15774, .F. ) ;
#13764 = ORIENTED_EDGE ( 'NONE', *, *, #13017, .F. ) ;
#13765 = ORIENTED_EDGE ( 'NONE', *, *, #11970, .T. ) ;
#13766 = AXIS2_PLACEMENT_3D ( 'NONE', #1985, #7380, #2231 ) ;
#13767 = ADVANCED_FACE ( 'NONE', ( #15194 ), #8583, .T. ) ;
#13768 = ORIENTED_EDGE ( 'NONE', *, *, #2151, .F. ) ;
#13769 = AXIS2_PLACEMENT_3D ( 'NONE', #2915, #8152, #13404 ) ;
#13770 = VECTOR ( 'NONE', #3588, 1000.000000000000000 ) ;
#13771 = VECTOR ( 'NONE', #10563, 1000.000000000000000 ) ;
#13772 = VERTEX_POINT ( 'NONE', #3259 ) ;
#13773 = ORIENTED_EDGE ( 'NONE', *, *, #7457, .F. ) ;
#13774 = CARTESIAN_POINT ( 'NONE',  ( -31.00000000000005329, 0.000000000000000000, 26.00000000000000000 ) ) ;
#13775 = DIRECTION ( 'NONE',  ( 1.000000000000000000, 0.000000000000000000, 0.000000000000000000 ) ) ;
#13776 = CARTESIAN_POINT ( 'NONE',  ( 22.99999999999999289, 68.00000000000000000, 37.00000000000002132 ) ) ;
#13777 = CIRCLE ( 'NONE', #619, 15.00000000000000000 ) ;
#13778 = CARTESIAN_POINT ( 'NONE',  ( -30.99999999999999645, 68.00000000000000000, -30.99999999999999289 ) ) ;
#13779 = CARTESIAN_POINT ( 'NONE',  ( 10.00000000000000000, 301.0487089519832011, -80.00000000000387956 ) ) ;
#13780 = EDGE_CURVE ( 'NONE', #1044, #8336, #6546, .T. ) ;
#13781 = DIRECTION ( 'NONE',  ( 1.000000000000000000, 0.000000000000000000, 3.854941057726246479E-16 ) ) ;
#13782 = VECTOR ( 'NONE', #15000, 1000.000000000000000 ) ;
#13783 = CARTESIAN_POINT ( 'NONE',  ( 0.000000000000000000, 0.000000000000000000, 0.000000000000000000 ) ) ;
#13784 = CIRCLE ( 'NONE', #3637, 20.75209553982835331 ) ;
#13785 = ORIENTED_EDGE ( 'NONE', *, *, #3362, .F. ) ;
#13786 = CARTESIAN_POINT ( 'NONE',  ( 31.99999999999998579, 10.00000000000000000, 22.99999999999999645 ) ) ;
#13787 = DIRECTION ( 'NONE',  ( 0.000000000000000000, 1.000000000000000000, 0.000000000000000000 ) ) ;
#13788 = DIRECTION ( 'NONE',  ( 1.141265444721583757E-16, -1.000000000000000000, 0.000000000000000000 ) ) ;
#13789 = DIRECTION ( 'NONE',  ( -0.000000000000000000, 0.09950371902100807464, -0.9950371902099882648 ) ) ;
#13791 = ORIENTED_EDGE ( 'NONE', *, *, #11865, .T. ) ;
#13790 = EDGE_LOOP ( 'NONE', ( #9756, #14889, #11914, #28 ) ) ;
#13792 = CONICAL_SURFACE ( 'NONE', #9129, 14.43750000000000000, 0.7483780475235185525 ) ;
#13793 = EDGE_CURVE ( 'NONE', #6668, #221, #7273, .T. ) ;
#13794 = LINE ( 'NONE', #2020, #6430 ) ;
#13795 =( NAMED_UNIT ( * ) PLANE_ANGLE_UNIT ( ) SI_UNIT ( $, .RADIAN. ) );
#13796 = VECTOR ( 'NONE', #13095, 1000.000000000000000 ) ;
#13797 = AXIS2_PLACEMENT_3D ( 'NONE', #9710, #13489, #2922 ) ;
#13798 = CARTESIAN_POINT ( 'NONE',  ( -55.99999999999989342, 473.6663340069158039, -575.6402177818052905 ) ) ;
#13799 = DIRECTION ( 'NONE',  ( -0.000000000000000000, -0.000000000000000000, 1.000000000000000000 ) ) ;
#13800 = ORIENTED_EDGE ( 'NONE', *, *, #12255, .F. ) ;
#13801 = DIRECTION ( 'NONE',  ( 1.000000000000000000, 0.000000000000000000, 0.000000000000000000 ) ) ;
#13802 = VECTOR ( 'NONE', #15324, 1000.000000000000000 ) ;
#13803 = DIRECTION ( 'NONE',  ( 0.000000000000000000, 0.000000000000000000, 1.000000000000000000 ) ) ;
#13805 = EDGE_CURVE ( 'NONE', #2869, #6725, #8496, .T. ) ;
#13804 = VERTEX_POINT ( 'NONE', #3430 ) ;
#13806 = CARTESIAN_POINT ( 'NONE',  ( 20.99999999999996092, 3.000000000000000000, 35.00000000000000711 ) ) ;
#13807 = EDGE_CURVE ( 'NONE', #4810, #985, #9869, .T. ) ;
#13808 = CARTESIAN_POINT ( 'NONE',  ( -40.00000000000000000, 68.00000000000000000, -25.99999999999999645 ) ) ;
#13809 = DIRECTION ( 'NONE',  ( 0.000000000000000000, 0.000000000000000000, 1.000000000000000000 ) ) ;
#13810 = VECTOR ( 'NONE', #5879, 1000.000000000000000 ) ;
#13811 = DIRECTION ( 'NONE',  ( -0.000000000000000000, 1.000000000000000000, -0.000000000000000000 ) ) ;
#13812 = VECTOR ( 'NONE', #10185, 1000.000000000000000 ) ;
#13813 = FACE_OUTER_BOUND ( 'NONE', #6487, .T. ) ;
#13814 = ORIENTED_EDGE ( 'NONE', *, *, #2646, .F. ) ;
#13815 = ADVANCED_FACE ( 'NONE', ( #4792 ), #7104, .T. ) ;
#13816 = ADVANCED_FACE ( 'NONE', ( #12527 ), #12067, .T. ) ;
#13817 = ADVANCED_FACE ( 'NONE', ( #685 ), #11156, .F. ) ;
#13818 = DIRECTION ( 'NONE',  ( -1.000000000000000000, -0.000000000000000000, -0.000000000000000000 ) ) ;
#13819 = EDGE_CURVE ( 'NONE', #6925, #6110, #14246, .T. ) ;
#13820 = CIRCLE ( 'NONE', #3399, 0.7366000000000039183 ) ;
#13821 = DIRECTION ( 'NONE',  ( 0.000000000000000000, 1.000000000000000000, 0.000000000000000000 ) ) ;
#13822 = ORIENTED_EDGE ( 'NONE', *, *, #12551, .T. ) ;
#13823 = CARTESIAN_POINT ( 'NONE',  ( 30.99999999999997513, 0.000000000000000000, 30.99999999999999645 ) ) ;
#13824 = AXIS2_PLACEMENT_3D ( 'NONE', #14190, #7815, #6431 ) ;
#13825 = ORIENTED_EDGE ( 'NONE', *, *, #3446, .F. ) ;
#13826 = AXIS2_PLACEMENT_3D ( 'NONE', #6813, #8283, #12071 ) ;
#13827 = CARTESIAN_POINT ( 'NONE',  ( 46.99999999999988631, 523.2161522479888163, -502.8936384967199729 ) ) ;
#13828 = FACE_OUTER_BOUND ( 'NONE', #7850, .T. ) ;
#13829 = ORIENTED_EDGE ( 'NONE', *, *, #7567, .T. ) ;
#13830 = CARTESIAN_POINT ( 'NONE',  ( -23.00000000000002487, 0.000000000000000000, -31.00000000000003553 ) ) ;
#13831 = AXIS2_PLACEMENT_3D ( 'NONE', #9772, #7003, #7246 ) ;
#13832 = DIRECTION ( 'NONE',  ( 1.000000000000000000, 0.000000000000000000, 0.000000000000000000 ) ) ;
#13833 = CARTESIAN_POINT ( 'NONE',  ( -2.220446049250313081E-13, 135.5000000000000000, 0.000000000000000000 ) ) ;
#13834 = ORIENTED_EDGE ( 'NONE', *, *, #5653, .T. ) ;
#13835 = VECTOR ( 'NONE', #3600, 1000.000000000000000 ) ;
#13836 = SURFACE_SIDE_STYLE ('',( #7292 ) ) ;
#13837 = DIRECTION ( 'NONE',  ( -1.000000000000000000, 0.000000000000000000, 3.854941057726251409E-16 ) ) ;
#13838 = ORIENTED_EDGE ( 'NONE', *, *, #13418, .F. ) ;
#13839 = EDGE_CURVE ( 'NONE', #15603, #3880, #16433, .T. ) ;
#13840 = ORIENTED_EDGE ( 'NONE', *, *, #6474, .T. ) ;
#13841 = EDGE_CURVE ( 'NONE', #11305, #9318, #8922, .T. ) ;
#13842 = CARTESIAN_POINT ( 'NONE',  ( 5.945602903476760126, 0.000000000000000000, 0.000000000000000000 ) ) ;
#13843 = EDGE_CURVE ( 'NONE', #7040, #10318, #14409, .T. ) ;
#13844 = AXIS2_PLACEMENT_3D ( 'NONE', #7549, #12974, #961 ) ;
#13845 = DIRECTION ( 'NONE',  ( -1.000000000000000000, -0.000000000000000000, -0.000000000000000000 ) ) ;
#13846 = ORIENTED_EDGE ( 'NONE', *, *, #12637, .T. ) ;
#13847 = CARTESIAN_POINT ( 'NONE',  ( -1.224646799147350495E-16, 41.00000000000000711, 6.000000000000000000 ) ) ;
#13848 = FACE_OUTER_BOUND ( 'NONE', #5279, .T. ) ;
#13849 = ORIENTED_EDGE ( 'NONE', *, *, #4757, .F. ) ;
#13850 = ORIENTED_EDGE ( 'NONE', *, *, #8705, .T. ) ;
#13851 = CARTESIAN_POINT ( 'NONE',  ( 40.00000000000000000, 68.00000000000000000, 26.00000000000000355 ) ) ;
#13852 = LINE ( 'NONE', #16419, #1289 ) ;
#13853 = VERTEX_POINT ( 'NONE', #11823 ) ;
#13854 = AXIS2_PLACEMENT_3D ( 'NONE', #12280, #13818, #4788 ) ;
#13855 = LINE ( 'NONE', #12390, #3937 ) ;
#13856 = VERTEX_POINT ( 'NONE', #6569 ) ;
#13857 = EDGE_LOOP ( 'NONE', ( #11125, #250, #15815, #6791 ) ) ;
#13858 = ORIENTED_EDGE ( 'NONE', *, *, #10805, .F. ) ;
#13859 = VERTEX_POINT ( 'NONE', #15606 ) ;
#13860 = ORIENTED_EDGE ( 'NONE', *, *, #2242, .T. ) ;
#13861 = CARTESIAN_POINT ( 'NONE',  ( -3.000000000000001776, 40.80057950988138771, 9.013878188659973034 ) ) ;
#13862 = TOROIDAL_SURFACE ( 'NONE', #2617, 4.695405383895982609, 9.000000000000000000 ) ;
#13863 = DIRECTION ( 'NONE',  ( 0.000000000000000000, 0.000000000000000000, -1.000000000000000000 ) ) ;
#13864 = CARTESIAN_POINT ( 'NONE',  ( -37.00000000000000000, 0.000000000000000000, 23.00000000000000355 ) ) ;
#13865 = DIRECTION ( 'NONE',  ( 0.000000000000000000, 0.000000000000000000, -1.000000000000000000 ) ) ;
#13866 = CARTESIAN_POINT ( 'NONE',  ( -55.99999999999989342, 523.2161522479893847, -595.2478186815853860 ) ) ;
#13867 = CARTESIAN_POINT ( 'NONE',  ( 18.99999999999998224, 8.000000000000000000, -39.99999999999999289 ) ) ;
#13868 = ADVANCED_FACE ( 'NONE', ( #2635, #15355 ), #4950, .T. ) ;
#13869 = DIRECTION ( 'NONE',  ( 6.123031769111888756E-17, -1.000000000000000000, -3.749151804555344967E-33 ) ) ;
#13870 = FACE_BOUND ( 'NONE', #14279, .T. ) ;
#13871 = ORIENTED_EDGE ( 'NONE', *, *, #14537, .F. ) ;
#13872 = DIRECTION ( 'NONE',  ( 5.551115123125781913E-15, 0.000000000000000000, -1.000000000000000000 ) ) ;
#13873 = DIRECTION ( 'NONE',  ( 0.000000000000000000, 0.000000000000000000, -1.000000000000000000 ) ) ;
#13874 = AXIS2_PLACEMENT_3D ( 'NONE', #8861, #3544, #7220 ) ;
#13875 = AXIS2_PLACEMENT_3D ( 'NONE', #14045, #11462, #16695 ) ;
#13876 = DIRECTION ( 'NONE',  ( 0.000000000000000000, 0.3853514969300962378, 0.9227698650333863162 ) ) ;
#13878 = VERTEX_POINT ( 'NONE', #3594 ) ;
#13877 = ORIENTED_EDGE ( 'NONE', *, *, #11970, .F. ) ;
#13879 = LINE ( 'NONE', #7161, #9759 ) ;
#13880 = ORIENTED_EDGE ( 'NONE', *, *, #15800, .T. ) ;
#13881 = DIRECTION ( 'NONE',  ( 1.000000000000000000, -0.000000000000000000, 0.000000000000000000 ) ) ;
#13882 = EDGE_CURVE ( 'NONE', #14413, #7396, #11657, .T. ) ;
#13883 = PLANE ( 'NONE',  #9081 ) ;
#13884 = DIRECTION ( 'NONE',  ( 0.000000000000000000, 0.000000000000000000, 1.000000000000000000 ) ) ;
#13885 = VECTOR ( 'NONE', #1815, 1000.000000000000000 ) ;
#13886 = ORIENTED_EDGE ( 'NONE', *, *, #15669, .F. ) ;
#13887 = VECTOR ( 'NONE', #15028, 1000.000000000000000 ) ;
#13888 = DIRECTION ( 'NONE',  ( 0.000000000000000000, 0.000000000000000000, 1.000000000000000000 ) ) ;
#13889 = ADVANCED_FACE ( 'NONE', ( #14160 ), #14317, .T. ) ;
#13890 = CARTESIAN_POINT ( 'NONE',  ( 1.286622718088548112E-12, 260.4765148507136701, 287.1312267635912008 ) ) ;
#13891 = ORIENTED_EDGE ( 'NONE', *, *, #13970, .F. ) ;
#13892 = DIRECTION ( 'NONE',  ( 0.000000000000000000, 0.000000000000000000, 1.000000000000000000 ) ) ;
#13893 = CARTESIAN_POINT ( 'NONE',  ( -2.764312543576791015, 191.4687391198920920, 37.59778641568981072 ) ) ;
#13894 = CARTESIAN_POINT ( 'NONE',  ( -31.81980515339462912, 0.000000000000000000, 31.81980515339465043 ) ) ;
#13895 = FACE_OUTER_BOUND ( 'NONE', #11195, .T. ) ;
#13896 = DIRECTION ( 'NONE',  ( -0.000000000000000000, 0.000000000000000000, 1.000000000000000000 ) ) ;
#13897 = ORIENTED_EDGE ( 'NONE', *, *, #8624, .T. ) ;
#13898 = VECTOR ( 'NONE', #6760, 1000.000000000000000 ) ;
#13899 = CARTESIAN_POINT ( 'NONE',  ( -13.11912225705329327, 0.000000000000000000, 0.000000000000000000 ) ) ;
#13900 = AXIS2_PLACEMENT_3D ( 'NONE', #14627, #11107, #4413 ) ;
#13901 = CARTESIAN_POINT ( 'NONE',  ( -45.00000000000000000, 549.5810598491746077, -518.1154249974242703 ) ) ;
#13902 = EDGE_CURVE ( 'NONE', #8973, #12698, #7611, .T. ) ;
#13903 = VERTEX_POINT ( 'NONE', #2380 ) ;
#13904 = EDGE_CURVE ( 'NONE', #16578, #7039, #8550, .T. ) ;
#13905 = ADVANCED_FACE ( 'NONE', ( #68 ), #10118, .F. ) ;
#13906 = DIRECTION ( 'NONE',  ( -0.000000000000000000, -1.000000000000000000, -0.000000000000000000 ) ) ;
#13907 = ORIENTED_EDGE ( 'NONE', *, *, #7338, .T. ) ;
#13908 = CARTESIAN_POINT ( 'NONE',  ( -26.00000000000000000, 19.00000000000000000, -31.00000000000003908 ) ) ;
#13909 = EDGE_CURVE ( 'NONE', #750, #14463, #15127, .T. ) ;
#13910 = VECTOR ( 'NONE', #12753, 1000.000000000000000 ) ;
#13911 = EDGE_CURVE ( 'NONE', #2045, #12055, #10376, .T. ) ;
#13912 = LINE ( 'NONE', #15283, #15532 ) ;
#13913 = ORIENTED_EDGE ( 'NONE', *, *, #2267, .F. ) ;
#13914 = VECTOR ( 'NONE', #15128, 1000.000000000000000 ) ;
#13915 = CARTESIAN_POINT ( 'NONE',  ( 30.99999999999999645, 3.000000000000000000, -25.99999999999999645 ) ) ;
#13916 = EDGE_CURVE ( 'NONE', #13331, #1995, #11288, .T. ) ;
#13917 = CARTESIAN_POINT ( 'NONE',  ( -2.220446049250313081E-13, 75.00000000000001421, 3.000000000000000000 ) ) ;
#13918 = CARTESIAN_POINT ( 'NONE',  ( 30.99999999999999645, 3.000000000000000000, 26.00000000000000355 ) ) ;
#13919 = VERTEX_POINT ( 'NONE', #13039 ) ;
#13920 = SURFACE_SIDE_STYLE ('',( #3443 ) ) ;
#13921 = DIRECTION ( 'NONE',  ( 0.000000000000000000, 1.000000000000000000, 0.000000000000000000 ) ) ;
#13922 = VERTEX_POINT ( 'NONE', #1180 ) ;
#13923 = VERTEX_POINT ( 'NONE', #6398 ) ;
#13924 = CARTESIAN_POINT ( 'NONE',  ( 394.0000000000001137, 449.3157724647196005, -155.1251505852266632 ) ) ;
#13925 = APPLICATION_PROTOCOL_DEFINITION ( 'draft international standard', 'automotive_design', 1998, #628 ) ;
#13926 = CIRCLE ( 'NONE', #6772, 6.473199999999998511 ) ;
#13927 = EDGE_CURVE ( 'NONE', #5619, #3270, #10204, .T. ) ;
#13928 = CARTESIAN_POINT ( 'NONE',  ( 1.507804506096818820, 62.60084458484482894, 9.381017998102993971 ) ) ;
#13929 = ORIENTED_EDGE ( 'NONE', *, *, #15894, .F. ) ;
#13930 = DIRECTION ( 'NONE',  ( -3.854941057726253874E-16, 0.000000000000000000, -1.000000000000000000 ) ) ;
#13931 = EDGE_CURVE ( 'NONE', #5761, #5602, #15685, .T. ) ;
#13932 = LINE ( 'NONE', #6094, #5041 ) ;
#13933 = ADVANCED_FACE ( 'NONE', ( #6484 ), #11483, .T. ) ;
#13934 = ADVANCED_FACE ( 'NONE', ( #1022 ), #10453, .T. ) ;
#13935 = ORIENTED_EDGE ( 'NONE', *, *, #1106, .F. ) ;
#13936 = PLANE ( 'NONE',  #13560 ) ;
#13937 = ADVANCED_FACE ( 'NONE', ( #10706 ), #4281, .F. ) ;
#13938 = CARTESIAN_POINT ( 'NONE',  ( -20.99999999999999645, 19.00000000000000000, -31.00000000000003908 ) ) ;
#13939 = EDGE_LOOP ( 'NONE', ( #2327, #9873, #5401, #9685 ) ) ;
#13940 = CIRCLE ( 'NONE', #15572, 22.50000000000000000 ) ;
#13941 = AXIS2_PLACEMENT_3D ( 'NONE', #14121, #8634, #13865 ) ;
#13942 = CARTESIAN_POINT ( 'NONE',  ( 7.000000000000000000, -17.85000000000000142, -2.225795557450314789E-15 ) ) ;
#13943 = VERTEX_POINT ( 'NONE', #1690 ) ;
#13944 = VERTEX_POINT ( 'NONE', #157 ) ;
#13945 = EDGE_LOOP ( 'NONE', ( #11794, #15732, #16345, #13613 ) ) ;
#13946 = PRODUCT_DEFINITION_CONTEXT ( 'detailed design', #76, 'design' ) ;
#13947 = EDGE_LOOP ( 'NONE', ( #15771, #10411, #10059, #2336 ) ) ;
#13948 = EDGE_LOOP ( 'NONE', ( #8148, #4028, #16785, #7170 ) ) ;
#13949 = DIRECTION ( 'NONE',  ( 0.000000000000000000, 0.000000000000000000, -1.000000000000000000 ) ) ;
#13950 = AXIS2_PLACEMENT_3D ( 'NONE', #13586, #609, #9805 ) ;
#13951 = DIRECTION ( 'NONE',  ( -0.000000000000000000, 1.000000000000000000, -0.000000000000000000 ) ) ;
#13952 = DIRECTION ( 'NONE',  ( 0.000000000000000000, 0.000000000000000000, -1.000000000000000000 ) ) ;
#13953 = CARTESIAN_POINT ( 'NONE',  ( -31.00000000000003197, 68.00000000000000000, -22.99999999999999645 ) ) ;
#13954 = CARTESIAN_POINT ( 'NONE',  ( -37.00000000000000000, 68.00000000000000000, 23.00000000000000355 ) ) ;
#13955 = CARTESIAN_POINT ( 'NONE',  ( 0.000000000000000000, 66.00000000000000000, 0.000000000000000000 ) ) ;
#13956 = DIRECTION ( 'NONE',  ( 1.000000000000000000, -0.000000000000000000, 0.000000000000000000 ) ) ;
#13957 = CARTESIAN_POINT ( 'NONE',  ( 31.81980515339464333, 11.00000000000000000, 35.11980515339463693 ) ) ;
#13958 = ORIENTED_EDGE ( 'NONE', *, *, #7989, .F. ) ;
#13959 = DIRECTION ( 'NONE',  ( 0.000000000000000000, -1.000000000000000000, 0.000000000000000000 ) ) ;
#13960 = DIRECTION ( 'NONE',  ( -0.000000000000000000, -1.000000000000000000, -0.000000000000000000 ) ) ;
#13961 = CARTESIAN_POINT ( 'NONE',  ( 55.99999999999989342, 559.9933750504617365, -546.7230258972048205 ) ) ;
#13963 = VERTEX_POINT ( 'NONE', #7009 ) ;
#13962 = VERTEX_POINT ( 'NONE', #8301 ) ;
#13964 = CARTESIAN_POINT ( 'NONE',  ( -31.00000000000000000, 11.00000000000000000, 30.99999999999999289 ) ) ;
#13965 = ADVANCED_FACE ( 'NONE', ( #13207 ), #6155, .F. ) ;
#13966 = DIRECTION ( 'NONE',  ( -1.000000000000000000, -0.000000000000000000, -0.000000000000000000 ) ) ;
#13967 = FACE_OUTER_BOUND ( 'NONE', #338, .T. ) ;
#13968 = DIRECTION ( 'NONE',  ( -0.000000000000000000, -1.000000000000000000, -0.000000000000000000 ) ) ;
#13969 = EDGE_LOOP ( 'NONE', ( #2152, #2401, #284, #10137 ) ) ;
#13970 = EDGE_CURVE ( 'NONE', #12012, #15132, #5642, .T. ) ;
#13971 = UNCERTAINTY_MEASURE_WITH_UNIT (LENGTH_MEASURE( 1.000000000000000082E-05 ), #11114, 'distance_accuracy_value', 'NONE');
#13972 = CARTESIAN_POINT ( 'NONE',  ( -55.99999999999989342, 549.5810598491746077, -531.8108303813202156 ) ) ;
#13973 = CARTESIAN_POINT ( 'NONE',  ( 1.231993379943791155E-12, 193.4898140233672450, 37.52989836422092651 ) ) ;
#13974 = ORIENTED_EDGE ( 'NONE', *, *, #10986, .T. ) ;
#13975 = CARTESIAN_POINT ( 'NONE',  ( -3.000000000000002220, 60.19966235751221006, 9.013878188659974811 ) ) ;
#13976 = CARTESIAN_POINT ( 'NONE',  ( -3.269999999997899920, 192.9645375484312524, 37.54886512656518249 ) ) ;
#13977 = DIRECTION ( 'NONE',  ( 0.000000000000000000, 0.9848077530122061329, 0.1736481776669406840 ) ) ;
#13978 = AXIS2_PLACEMENT_3D ( 'NONE', #8419, #16391, #9954 ) ;
#13979 = FACE_OUTER_BOUND ( 'NONE', #2837, .T. ) ;
#13980 = DIRECTION ( 'NONE',  ( -1.000000000000000000, -0.000000000000000000, -8.673617379884027583E-16 ) ) ;
#13981 = ORIENTED_EDGE ( 'NONE', *, *, #13819, .F. ) ;
#13982 = FACE_OUTER_BOUND ( 'NONE', #13247, .T. ) ;
#13983 = EDGE_CURVE ( 'NONE', #1948, #1911, #1527, .T. ) ;
#13984 = DIRECTION ( 'NONE',  ( 1.000000000000000000, 0.000000000000000000, 0.000000000000000000 ) ) ;
#13985 = DIRECTION ( 'NONE',  ( -0.000000000000000000, -1.000000000000000000, 0.000000000000000000 ) ) ;
#13986 = AXIS2_PLACEMENT_3D ( 'NONE', #11480, #10372, #14156 ) ;
#13987 = EDGE_LOOP ( 'NONE', ( #5158, #9452, #14690, #13467 ) ) ;
#13988 = CIRCLE ( 'NONE', #3571, 4.999999999999997335 ) ;
#13989 = DIRECTION ( 'NONE',  ( 0.000000000000000000, 1.000000000000000000, 7.137148015447440312E-15 ) ) ;
#13990 = DIRECTION ( 'NONE',  ( 0.000000000000000000, -0.3746065934159052424, 0.9271838545667901998 ) ) ;
#13991 = ORIENTED_EDGE ( 'NONE', *, *, #16025, .T. ) ;
#13992 = DIRECTION ( 'NONE',  ( 0.000000000000000000, 0.000000000000000000, -1.000000000000000000 ) ) ;
#13993 =( GEOMETRIC_REPRESENTATION_CONTEXT ( 3 ) GLOBAL_UNCERTAINTY_ASSIGNED_CONTEXT ( ( #8240 ) ) GLOBAL_UNIT_ASSIGNED_CONTEXT ( ( #11087, #16574, #11499 ) ) REPRESENTATION_CONTEXT ( 'NONE', 'WORKASPACE' ) );
#13994 = CARTESIAN_POINT ( 'NONE',  ( -26.00000000000001776, 10.00000000000000000, 33.00000000000000711 ) ) ;
#13995 = CARTESIAN_POINT ( 'NONE',  ( -36.00000000000000711, 8.000000000000000000, -19.00000000000000000 ) ) ;
#13996 = ORIENTED_EDGE ( 'NONE', *, *, #16780, .T. ) ;
#13997 = EDGE_CURVE ( 'NONE', #5558, #11568, #16122, .T. ) ;
#13998 = DIRECTION ( 'NONE',  ( 0.000000000000000000, -0.9950371902099846011, -0.09950371902104368504 ) ) ;
#13999 = CARTESIAN_POINT ( 'NONE',  ( 0.000000000000000000, 19.00100000000000122, 0.000000000000000000 ) ) ;
#14000 = DIRECTION ( 'NONE',  ( -1.000000000000000000, 0.000000000000000000, 0.000000000000000000 ) ) ;
#14001 = ORIENTED_EDGE ( 'NONE', *, *, #5398, .F. ) ;
#14002 = AXIS2_PLACEMENT_3D ( 'NONE', #1043, #13068, #6593 ) ;
#14003 = LINE ( 'NONE', #4633, #13020 ) ;
#14004 = AXIS2_PLACEMENT_3D ( 'NONE', #1857, #3230, #14825 ) ;
#14005 = APPLICATION_PROTOCOL_DEFINITION ( 'draft international standard', 'automotive_design', 1998, #5664 ) ;
#14006 = EDGE_CURVE ( 'NONE', #1082, #7330, #9338, .T. ) ;
#14007 = CARTESIAN_POINT ( 'NONE',  ( -26.00000000000002842, 0.000000000000000000, 34.00000000000000711 ) ) ;
#14008 = VERTEX_POINT ( 'NONE', #499 ) ;
#14009 = DIRECTION ( 'NONE',  ( -0.000000000000000000, -0.000000000000000000, 1.000000000000000000 ) ) ;
#14010 = DIRECTION ( 'NONE',  ( -0.000000000000000000, 1.000000000000000000, -0.000000000000000000 ) ) ;
#14011 = CIRCLE ( 'NONE', #5504, 13.69540538389601991 ) ;
#14012 = VERTEX_POINT ( 'NONE', #4768 ) ;
#14013 = DIRECTION ( 'NONE',  ( 0.000000000000000000, 0.000000000000000000, -1.000000000000000000 ) ) ;
#14014 =( REPRESENTATION_RELATIONSHIP ('NONE','NONE', #15277, #1329 ) REPRESENTATION_RELATIONSHIP_WITH_TRANSFORMATION ( #11094 )SHAPE_REPRESENTATION_RELATIONSHIP( ) );
#14015 = CARTESIAN_POINT ( 'NONE',  ( 31.00000000000000711, 68.00000000000000000, -30.99999999999999289 ) ) ;
#14016 = VERTEX_POINT ( 'NONE', #579 ) ;
#14017 = EDGE_CURVE ( 'NONE', #15832, #1196, #9666, .T. ) ;
#14018 =( LENGTH_UNIT ( ) NAMED_UNIT ( * ) SI_UNIT ( .MILLI., .METRE. ) );
#14019 = VERTEX_POINT ( 'NONE', #8734 ) ;
#14020 = ORIENTED_EDGE ( 'NONE', *, *, #3913, .T. ) ;
#14021 = EDGE_LOOP ( 'NONE', ( #9462, #3822, #16055, #13283 ) ) ;
#14022 = EDGE_CURVE ( 'NONE', #11869, #12394, #11295, .T. ) ;
#14023 = EDGE_CURVE ( 'NONE', #5336, #14967, #8400, .T. ) ;
#14024 = AXIS2_PLACEMENT_3D ( 'NONE', #8019, #46, #1159 ) ;
#14025 = EDGE_CURVE ( 'NONE', #4477, #1411, #4438, .T. ) ;
#14026 = EDGE_CURVE ( 'NONE', #12863, #2782, #6892, .T. ) ;
#14027 = ORIENTED_EDGE ( 'NONE', *, *, #4134, .F. ) ;
#14028 = ORIENTED_EDGE ( 'NONE', *, *, #9516, .T. ) ;
#14029 = CARTESIAN_POINT ( 'NONE',  ( -55.99999999999988631, 658.4713480608917280, -425.4301204538002139 ) ) ;
#14030 = CARTESIAN_POINT ( 'NONE',  ( -440.0000000000000568, 425.7506394335853201, 109.9999999999999858 ) ) ;
#14031 = DIRECTION ( 'NONE',  ( 0.000000000000000000, -0.000000000000000000, 1.000000000000000000 ) ) ;
#14032 = DIRECTION ( 'NONE',  ( -1.000000000000000000, -0.000000000000000000, -0.000000000000000000 ) ) ;
#14033 = CARTESIAN_POINT ( 'NONE',  ( 3.000000000000000000, 41.00000000000000711, 6.000000000000000000 ) ) ;
#14034 = AXIS2_PLACEMENT_3D ( 'NONE', #11701, #11781, #16928 ) ;
#14035 = DIRECTION ( 'NONE',  ( 1.000000000000000000, 0.000000000000000000, -0.000000000000000000 ) ) ;
#14036 = CARTESIAN_POINT ( 'NONE',  ( 25.99999999999999645, 68.00000000000000000, 40.00000000000002132 ) ) ;
#14037 = VERTEX_POINT ( 'NONE', #831 ) ;
#14038 = DIRECTION ( 'NONE',  ( 0.000000000000000000, 1.000000000000000000, 0.000000000000000000 ) ) ;
#14039 = DIRECTION ( 'NONE',  ( -1.000000000000000000, -0.000000000000000000, -0.000000000000000000 ) ) ;
#14040 = VECTOR ( 'NONE', #1448, 1000.000000000000000 ) ;
#14041 = STYLED_ITEM ( 'NONE', ( #16202 ), #14050 ) ;
#14042 = DIRECTION ( 'NONE',  ( 0.000000000000000000, 0.000000000000000000, -1.000000000000000000 ) ) ;
#14044 = VERTEX_POINT ( 'NONE', #16533 ) ;
#14043 = ORIENTED_EDGE ( 'NONE', *, *, #13807, .T. ) ;
#14045 = CARTESIAN_POINT ( 'NONE',  ( 394.0000000000001137, 339.3157724647196005, -104.9456657433597968 ) ) ;
#14046 = ADVANCED_FACE ( 'NONE', ( #6050 ), #9777, .T. ) ;
#14047 = ORIENTED_EDGE ( 'NONE', *, *, #924, .F. ) ;
#14048 = AXIS2_PLACEMENT_3D ( 'NONE', #12286, #9874, #3184 ) ;
#14049 = DIRECTION ( 'NONE',  ( -1.000000000000000000, -0.000000000000000000, -0.000000000000000000 ) ) ;
#14050 = MANIFOLD_SOLID_BREP ( 'Imported1', #15945 ) ;
#14051 = CARTESIAN_POINT ( 'NONE',  ( 435.7731165870194445, 329.6061121441327941, -10.00000000000000000 ) ) ;
#14052 = DIRECTION ( 'NONE',  ( -0.000000000000000000, -1.000000000000000000, -0.000000000000000000 ) ) ;
#14053 = ORIENTED_EDGE ( 'NONE', *, *, #12860, .T. ) ;
#14054 = CIRCLE ( 'NONE', #885, 9.000000000000007105 ) ;
#14055 = DIRECTION ( 'NONE',  ( 1.000000000000000000, -0.000000000000000000, 4.956352788505159323E-16 ) ) ;
#14056 = DIRECTION ( 'NONE',  ( 1.000000000000000000, 0.000000000000000000, 0.000000000000000000 ) ) ;
#14057 = ORIENTED_EDGE ( 'NONE', *, *, #11492, .T. ) ;
#14058 = LINE ( 'NONE', #7675, #561 ) ;
#14059 = CARTESIAN_POINT ( 'NONE',  ( -55.99999999999988631, 173.0499717945046996, 146.7982946275220968 ) ) ;
#14060 = CARTESIAN_POINT ( 'NONE',  ( -31.81980515339462912, 8.000000000000000000, 31.81980515339465043 ) ) ;
#14061 = CIRCLE ( 'NONE', #1171, 4.695405383896011919 ) ;
#14062 = LINE ( 'NONE', #16880, #10524 ) ;
#14063 = DIRECTION ( 'NONE',  ( 0.000000000000000000, 0.000000000000000000, -1.000000000000000000 ) ) ;
#14064 = ORIENTED_EDGE ( 'NONE', *, *, #10037, .F. ) ;
#14065 = DIRECTION ( 'NONE',  ( -0.000000000000000000, -1.000000000000000000, -0.000000000000000000 ) ) ;
#14066 = TOROIDAL_SURFACE ( 'NONE', #3367, 4.695405383895982609, 9.000000000000000000 ) ;
#14067 = DIRECTION ( 'NONE',  ( 1.000000000000000000, -0.000000000000000000, -0.000000000000000000 ) ) ;
#14068 = PRESENTATION_STYLE_ASSIGNMENT (( #6070 ) ) ;
#14069 = AXIS2_PLACEMENT_3D ( 'NONE', #10257, #7833, #15575 ) ;
#14070 = VERTEX_POINT ( 'NONE', #4531 ) ;
#14071 = CARTESIAN_POINT ( 'NONE',  ( -26.00000000000002132, 10.00000000000000000, -39.99999999999999289 ) ) ;
#14072 = CIRCLE ( 'NONE', #13261, 2.999999999999995559 ) ;
#14073 = FACE_OUTER_BOUND ( 'NONE', #16769, .T. ) ;
#14074 = EDGE_LOOP ( 'NONE', ( #14434, #10678, #15720, #6852 ) ) ;
#14075 = DIRECTION ( 'NONE',  ( 0.000000000000000000, 0.000000000000000000, -1.000000000000000000 ) ) ;
#14076 = CIRCLE ( 'NONE', #6657, 4.999999999999997335 ) ;
#14077 = CIRCLE ( 'NONE', #14633, 9.000000000000007105 ) ;
#14078 = MANIFOLD_SOLID_BREP ( 'Cut-Extrude1', #3621 ) ;
#14079 = LINE ( 'NONE', #12869, #9848 ) ;
#14080 = CARTESIAN_POINT ( 'NONE',  ( 10.00000000000000000, 340.8211049126788907, -341.7267989266199493 ) ) ;
#14081 = ORIENTED_EDGE ( 'NONE', *, *, #13604, .F. ) ;
#14082 = LINE ( 'NONE', #11669, #1117 ) ;
#14083 = SURFACE_STYLE_USAGE ( .BOTH. , #15210 ) ;
#14084 = CARTESIAN_POINT ( 'NONE',  ( 0.2121372864215120557, 289.4599085936700931, 37.56312099760677370 ) ) ;
#14085 = ORIENTED_EDGE ( 'NONE', *, *, #15292, .T. ) ;
#14086 = AXIS2_PLACEMENT_3D ( 'NONE', #7718, #16830, #8947 ) ;
#14087 = CARTESIAN_POINT ( 'NONE',  ( -39.99999999999999289, 11.00000000000000000, 25.99999999999999645 ) ) ;
#14088 = VECTOR ( 'NONE', #4823, 1000.000000000000000 ) ;
#14089 = CIRCLE ( 'NONE', #5295, 35.00000000000000711 ) ;
#14090 = VECTOR ( 'NONE', #16271, 1000.000000000000000 ) ;
#14091 = DIRECTION ( 'NONE',  ( -0.000000000000000000, -1.000000000000000000, -0.000000000000000000 ) ) ;
#14092 = ORIENTED_EDGE ( 'NONE', *, *, #5935, .T. ) ;
#14093 = ADVANCED_FACE ( 'NONE', ( #7668 ), #7417, .F. ) ;
#14094 = VECTOR ( 'NONE', #9038, 1000.000000000000000 ) ;
#14095 = LINE ( 'NONE', #15713, #1713 ) ;
#14096 = CYLINDRICAL_SURFACE ( 'NONE', #9178, 3.000000000000002665 ) ;
#14097 = AXIS2_PLACEMENT_3D ( 'NONE', #9629, #9459, #8166 ) ;
#14098 = CARTESIAN_POINT ( 'NONE',  ( 46.99999999999988631, 549.5810598491749488, -570.6352214130889706 ) ) ;
#14099 = ORIENTED_EDGE ( 'NONE', *, *, #9102, .T. ) ;
#14100 = DIRECTION ( 'NONE',  ( 0.000000000000000000, 0.000000000000000000, -1.000000000000000000 ) ) ;
#14101 = LINE ( 'NONE', #2159, #10041 ) ;
#14102 = ORIENTED_EDGE ( 'NONE', *, *, #15169, .F. ) ;
#14103 = COLOUR_RGB ( '', 0.08235294, 0.09019608, 0.10196078) ;
#14104 = EDGE_CURVE ( 'NONE', #4853, #10521, #1962, .T. ) ;
#14105 = CARTESIAN_POINT ( 'NONE',  ( 10.00000000000000000, 376.0487089519837127, -155.0000000000033253 ) ) ;
#14106 = AXIS2_PLACEMENT_3D ( 'NONE', #4725, #13603, #12384 ) ;
#14107 = ORIENTED_EDGE ( 'NONE', *, *, #12641, .F. ) ;
#14108 = ORIENTED_EDGE ( 'NONE', *, *, #5992, .T. ) ;
#14109 = CARTESIAN_POINT ( 'NONE',  ( -26.00000000000001776, 8.000000000000000000, 33.00000000000000711 ) ) ;
#14110 = VECTOR ( 'NONE', #6087, 1000.000000000000000 ) ;
#14111 = MANIFOLD_SOLID_BREP ( 'Cut-Extrude1', #4968 ) ;
#14112 = ORIENTED_EDGE ( 'NONE', *, *, #3264, .F. ) ;
#14113 = ORIENTED_EDGE ( 'NONE', *, *, #6223, .T. ) ;
#14114 = EDGE_LOOP ( 'NONE', ( #13176, #12622, #6522, #9753 ) ) ;
#14115 = AXIS2_PLACEMENT_3D ( 'NONE', #2415, #16757, #4988 ) ;
#14116 = EDGE_CURVE ( 'NONE', #7040, #1685, #5240, .T. ) ;
#14117 = AXIS2_PLACEMENT_3D ( 'NONE', #11223, #11392, #7343 ) ;
#14118 = FACE_OUTER_BOUND ( 'NONE', #2160, .T. ) ;
#14119 = EDGE_CURVE ( 'NONE', #10179, #16083, #8290, .T. ) ;
#14120 = CARTESIAN_POINT ( 'NONE',  ( 1.574999999999999956, 0.000000000000000000, 0.000000000000000000 ) ) ;
#14121 = CARTESIAN_POINT ( 'NONE',  ( 35.00000000000000711, 0.000000000000000000, -35.00000000000000711 ) ) ;
#14122 = CIRCLE ( 'NONE', #3988, 22.50000000000000000 ) ;
#14123 = CARTESIAN_POINT ( 'NONE',  ( 394.0000000000001137, 341.5974953295075807, -105.4170192159777031 ) ) ;
#14124 = FACE_OUTER_BOUND ( 'NONE', #12623, .T. ) ;
#14125 = VECTOR ( 'NONE', #16135, 1000.000000000000000 ) ;
#14126 = EDGE_CURVE ( 'NONE', #6025, #7981, #10432, .T. ) ;
#14127 = ADVANCED_FACE ( 'NONE', ( #2620 ), #14221, .T. ) ;
#14128 = EDGE_CURVE ( 'NONE', #12822, #9226, #16871, .T. ) ;
#14129 = DIRECTION ( 'NONE',  ( 0.000000000000000000, 0.6427876096865299260, 0.7660444431189857850 ) ) ;
#14130 = EDGE_CURVE ( 'NONE', #7276, #4858, #13784, .T. ) ;
#14131 = CARTESIAN_POINT ( 'NONE',  ( -31.00000000000001776, 10.00000000000000000, 31.00000000000000000 ) ) ;
#14132 = ORIENTED_EDGE ( 'NONE', *, *, #11385, .T. ) ;
#14133 = DIRECTION ( 'NONE',  ( 1.000000000000000000, 0.000000000000000000, 0.000000000000000000 ) ) ;
#14134 = DIRECTION ( 'NONE',  ( 0.000000000000000000, 0.000000000000000000, 1.000000000000000000 ) ) ;
#14135 = VERTEX_POINT ( 'NONE', #15514 ) ;
#14136 = CARTESIAN_POINT ( 'NONE',  ( 10.00000000000000000, 0.000000000000000000, -206.3519347178565795 ) ) ;
#14138 = EDGE_LOOP ( 'NONE', ( #2169, #966 ) ) ;
#14137 = VERTEX_POINT ( 'NONE', #2358 ) ;
#14139 = CARTESIAN_POINT ( 'NONE',  ( 0.000000000000000000, -3.000000000000000000, 0.000000000000000000 ) ) ;
#14140 = VECTOR ( 'NONE', #5803, 1000.000000000000000 ) ;
#14141 = FACE_BOUND ( 'NONE', #10686, .T. ) ;
#14142 = DIRECTION ( 'NONE',  ( -0.000000000000000000, -0.000000000000000000, 1.000000000000000000 ) ) ;
#14143 = CYLINDRICAL_SURFACE ( 'NONE', #10782, 10.00000000000000178 ) ;
#14144 = ORIENTED_EDGE ( 'NONE', *, *, #1227, .T. ) ;
#14145 = UNCERTAINTY_MEASURE_WITH_UNIT (LENGTH_MEASURE( 1.000000000000000082E-05 ), #303, 'distance_accuracy_value', 'NONE');
#14146 = CARTESIAN_POINT ( 'NONE',  ( -31.81980515339462912, 8.000000000000000000, 31.81980515339465043 ) ) ;
#14147 = EDGE_CURVE ( 'NONE', #13919, #4673, #10217, .T. ) ;
#14148 = ADVANCED_FACE ( 'NONE', ( #3823 ), #2439, .F. ) ;
#14149 = ORIENTED_EDGE ( 'NONE', *, *, #8088, .F. ) ;
#14150 = CARTESIAN_POINT ( 'NONE',  ( -37.00000000000000711, 0.000000000000000000, 23.00000000000000000 ) ) ;
#14151 = VECTOR ( 'NONE', #393, 1000.000000000000114 ) ;
#14152 = ADVANCED_FACE ( 'NONE', ( #8904, #14296, #2526, #7756, #14141, #13019 ), #1248, .F. ) ;
#14153 = LINE ( 'NONE', #7677, #9791 ) ;
#14154 = LINE ( 'NONE', #2537, #1434 ) ;
#14155 = DIRECTION ( 'NONE',  ( 0.000000000000000000, 0.000000000000000000, -1.000000000000000000 ) ) ;
#14156 = DIRECTION ( 'NONE',  ( 1.000000000000000000, 0.000000000000000000, -0.000000000000000000 ) ) ;
#14157 = ORIENTED_EDGE ( 'NONE', *, *, #11283, .F. ) ;
#14158 = CARTESIAN_POINT ( 'NONE',  ( 56.72999999999999687, 183.8715257629570203, -18.38715257629581856 ) ) ;
#14159 = VECTOR ( 'NONE', #13420, 1000.000000000000000 ) ;
#14160 = FACE_OUTER_BOUND ( 'NONE', #454, .T. ) ;
#14161 = AXIS2_PLACEMENT_3D ( 'NONE', #9435, #11925, #9604 ) ;
#14162 = CARTESIAN_POINT ( 'NONE',  ( -1.224646799147350495E-16, 41.00000000000000711, 6.000000000000000000 ) ) ;
#14163 = ORIENTED_EDGE ( 'NONE', *, *, #7997, .F. ) ;
#14164 = DIRECTION ( 'NONE',  ( 6.123031769111888756E-17, 0.000000000000000000, 1.000000000000000000 ) ) ;
#14165 = CARTESIAN_POINT ( 'NONE',  ( -1.836909530733565148E-16, 6.000000000000000000, 3.000000000000000000 ) ) ;
#14166 = ORIENTED_EDGE ( 'NONE', *, *, #2667, .F. ) ;
#14167 = DIRECTION ( 'NONE',  ( 1.000000000000000000, -0.000000000000000000, -0.000000000000000000 ) ) ;
#14168 = MANIFOLD_SOLID_BREP ( 'Boss-Extrude1', #2502 ) ;
#14169 = DIRECTION ( 'NONE',  ( 0.000000000000000000, 1.000000000000000000, 0.000000000000000000 ) ) ;
#14170 = LINE ( 'NONE', #1192, #15259 ) ;
#14171 = ORIENTED_EDGE ( 'NONE', *, *, #13902, .F. ) ;
#14172 = AXIS2_PLACEMENT_3D ( 'NONE', #16212, #252, #10900 ) ;
#14173 = VECTOR ( 'NONE', #3127, 1000.000000000000000 ) ;
#14174 = CARTESIAN_POINT ( 'NONE',  ( 35.00000000000003553, -20.00000000000000000, -23.50000000000000000 ) ) ;
#14175 = CARTESIAN_POINT ( 'NONE',  ( 415.3629108289414944, 306.8565854934392974, 0.000000000000000000 ) ) ;
#14176 = DIRECTION ( 'NONE',  ( 1.000000000000000000, 0.000000000000000000, 0.000000000000000000 ) ) ;
#14177 = ORIENTED_EDGE ( 'NONE', *, *, #9913, .F. ) ;
#14178 = FACE_BOUND ( 'NONE', #3714, .T. ) ;
#14179 = ADVANCED_FACE ( 'NONE', ( #4163, #5620, #5361 ), #9498, .F. ) ;
#14180 = AXIS2_PLACEMENT_3D ( 'NONE', #8469, #13707, #1929 ) ;
#14181 = ORIENTED_EDGE ( 'NONE', *, *, #770, .T. ) ;
#14182 = AXIS2_PLACEMENT_3D ( 'NONE', #13725, #15178, #3414 ) ;
#14183 = DIRECTION ( 'NONE',  ( 1.000000000000000000, 0.000000000000000000, 0.000000000000000000 ) ) ;
#14184 = CARTESIAN_POINT ( 'NONE',  ( 39.75350601975127063, 301.2117639810886089, 0.000000000000000000 ) ) ;
#14185 = ADVANCED_FACE ( 'NONE', ( #138 ), #1593, .F. ) ;
#14186 = LINE ( 'NONE', #2487, #10709 ) ;
#14187 = ORIENTED_EDGE ( 'NONE', *, *, #1939, .T. ) ;
#14188 = CARTESIAN_POINT ( 'NONE',  ( -45.00000000000000000, 549.5810598491749488, -575.3306267969850296 ) ) ;
#14189 = ORIENTED_EDGE ( 'NONE', *, *, #6138, .F. ) ;
#14190 = CARTESIAN_POINT ( 'NONE',  ( -34.99999999999998579, -20.00000000000000000, 21.00000000000000355 ) ) ;
#14191 = ORIENTED_EDGE ( 'NONE', *, *, #6489, .T. ) ;
#14192 = VERTEX_POINT ( 'NONE', #14819 ) ;
#14193 = CIRCLE ( 'NONE', #11722, 3.300000000000025135 ) ;
#14194 = CARTESIAN_POINT ( 'NONE',  ( 394.0000000000001137, 240.7889724647196488, -104.2090657433598011 ) ) ;
#14195 = PRODUCT_DEFINITION ( 'UNKNOWN', '', #16589, #4206 ) ;
#14196 = ORIENTED_EDGE ( 'NONE', *, *, #15169, .T. ) ;
#14197 = DIRECTION ( 'NONE',  ( 1.000000000000000000, 0.000000000000000000, 0.000000000000000000 ) ) ;
#14198 = ORIENTED_EDGE ( 'NONE', *, *, #3756, .T. ) ;
#14199 = ADVANCED_FACE ( 'NONE', ( #4083 ), #1508, .T. ) ;
#14200 = ORIENTED_EDGE ( 'NONE', *, *, #13390, .T. ) ;
#14201 = B_SPLINE_CURVE_WITH_KNOTS ( 'NONE', 3,
 ( #16381, #7169, #12429, #4777, #6617, #13973 ),
 .UNSPECIFIED., .F., .F.,
 ( 4, 2, 4 ),
 ( 0.000000000000000000, 0.5000000000000000000, 1.000000000000000000 ),
 .UNSPECIFIED. ) ;
#14202 = CARTESIAN_POINT ( 'NONE',  ( -55.99999999999989342, 523.2161522479888163, -502.8936384967199729 ) ) ;
#14203 = DIRECTION ( 'NONE',  ( 0.000000000000000000, 0.000000000000000000, -1.000000000000000000 ) ) ;
#14204 = ORIENTED_EDGE ( 'NONE', *, *, #2335, .F. ) ;
#14205 = LINE ( 'NONE', #16931, #1745 ) ;
#14206 = DIRECTION ( 'NONE',  ( -0.000000000000000000, -1.000000000000000000, -0.000000000000000000 ) ) ;
#14207 = PLANE ( 'NONE',  #6574 ) ;
#14208 = DIRECTION ( 'NONE',  ( -0.000000000000000000, -0.000000000000000000, 1.000000000000000000 ) ) ;
#14209 = ORIENTED_EDGE ( 'NONE', *, *, #2254, .F. ) ;
#14210 = CARTESIAN_POINT ( 'NONE',  ( 34.00000000000002842, 0.000000000000000000, 23.00000000000000355 ) ) ;
#14211 = CARTESIAN_POINT ( 'NONE',  ( 25.99999999999997513, 10.00000000000000000, 31.00000000000003553 ) ) ;
#14212 = ORIENTED_EDGE ( 'NONE', *, *, #1734, .F. ) ;
#14213 = EDGE_CURVE ( 'NONE', #2814, #199, #16012, .T. ) ;
#14214 = CARTESIAN_POINT ( 'NONE',  ( -30.99999999999999289, 68.00000000000000000, 31.00000000000000000 ) ) ;
#14215 = VERTEX_POINT ( 'NONE', #15842 ) ;
#14216 = CARTESIAN_POINT ( 'NONE',  ( 0.000000000000000000, 240.7889724647196488, -110.6822657433598067 ) ) ;
#14217 = VECTOR ( 'NONE', #10917, 1000.000000000000000 ) ;
#14218 = EDGE_LOOP ( 'NONE', ( #10844, #8960, #3883, #9552 ) ) ;
#14219 = EDGE_CURVE ( 'NONE', #16915, #14244, #6810, .T. ) ;
#14220 = EDGE_LOOP ( 'NONE', ( #8874, #10794, #8703, #15260, #3033, #5175 ) ) ;
#14221 = PLANE ( 'NONE',  #1984 ) ;
#14222 = CARTESIAN_POINT ( 'NONE',  ( -26.00000000000000355, 19.00000000000000000, 31.00000000000003197 ) ) ;
#14223 = LINE ( 'NONE', #1002, #9426 ) ;
#14224 = ORIENTED_EDGE ( 'NONE', *, *, #14755, .T. ) ;
#14225 = CARTESIAN_POINT ( 'NONE',  ( 394.0000000000001137, 240.0523724647196389, -17.15546574335979813 ) ) ;
#14226 = EDGE_LOOP ( 'NONE', ( #14611, #2762, #6286, #7749, #10010, #3214 ) ) ;
#14227 = DIRECTION ( 'NONE',  ( 0.000000000000000000, 0.000000000000000000, -1.000000000000000000 ) ) ;
#14228 = VECTOR ( 'NONE', #10383, 1000.000000000000114 ) ;
#14229 = LINE ( 'NONE', #2287, #11978 ) ;
#14230 = CARTESIAN_POINT ( 'NONE',  ( 7.000000000000001776, 0.000000000000000000, -75.00000000000000000 ) ) ;
#14231 = EDGE_CURVE ( 'NONE', #9832, #4632, #12157, .T. ) ;
#14232 = FACE_OUTER_BOUND ( 'NONE', #12109, .T. ) ;
#14233 = EDGE_CURVE ( 'NONE', #16590, #8336, #1332, .T. ) ;
#14234 = DIRECTION ( 'NONE',  ( 1.000000000000000000, 0.000000000000000000, 0.000000000000000000 ) ) ;
#14236 = ORIENTED_EDGE ( 'NONE', *, *, #7526, .T. ) ;
#14235 = ORIENTED_EDGE ( 'NONE', *, *, #2434, .T. ) ;
#14237 = DIRECTION ( 'NONE',  ( 0.000000000000000000, 0.000000000000000000, 1.000000000000000000 ) ) ;
#14238 = ADVANCED_FACE ( 'NONE', ( #14560 ), #2783, .F. ) ;
#14239 = EDGE_CURVE ( 'NONE', #747, #13878, #14737, .T. ) ;
#14240 = EDGE_CURVE ( 'NONE', #5928, #15603, #10517, .T. ) ;
#14241 = CARTESIAN_POINT ( 'NONE',  ( -46.99999999999988631, 523.2161522479888163, -502.8936384967199729 ) ) ;
#14242 = ADVANCED_FACE ( 'NONE', ( #14478 ), #224, .T. ) ;
#14243 = CARTESIAN_POINT ( 'NONE',  ( 22.99999999999998224, 10.00000000000000000, -31.00000000000003197 ) ) ;
#14244 = VERTEX_POINT ( 'NONE', #8629 ) ;
#14245 = DIRECTION ( 'NONE',  ( 0.000000000000000000, 0.000000000000000000, 1.000000000000000000 ) ) ;
#14246 = CIRCLE ( 'NONE', #6826, 13.69540538389598439 ) ;
#14247 = CARTESIAN_POINT ( 'NONE',  ( 414.6791312654406738, 352.3556387948262341, 0.000000000000000000 ) ) ;
#14248 = ORIENTED_EDGE ( 'NONE', *, *, #3732, .T. ) ;
#14249 = DIRECTION ( 'NONE',  ( 0.000000000000000000, 0.000000000000000000, 1.000000000000000000 ) ) ;
#14250 = DIRECTION ( 'NONE',  ( 0.000000000000000000, 0.000000000000000000, 1.000000000000000000 ) ) ;
#14251 = PLANE ( 'NONE',  #11963 ) ;
#14252 = VERTEX_POINT ( 'NONE', #13535 ) ;
#14253 = LINE ( 'NONE', #12711, #10158 ) ;
#14254 = DIRECTION ( 'NONE',  ( 1.000000000000000000, 0.000000000000000000, 0.000000000000000000 ) ) ;
#14255 = EDGE_LOOP ( 'NONE', ( #13907, #7151 ) ) ;
#14256 = CARTESIAN_POINT ( 'NONE',  ( -46.99999999999988631, 473.6663340069157471, -531.5012393965008641 ) ) ;
#14257 = AXIS2_PLACEMENT_3D ( 'NONE', #179, #10642, #13226 ) ;
#14258 =( NAMED_UNIT ( * ) PLANE_ANGLE_UNIT ( ) SI_UNIT ( $, .RADIAN. ) );
#14259 = EDGE_CURVE ( 'NONE', #12986, #12394, #7185, .T. ) ;
#14260 = ORIENTED_EDGE ( 'NONE', *, *, #16170, .T. ) ;
#14261 = CARTESIAN_POINT ( 'NONE',  ( -440.0000000000000568, 620.7506394335853201, -11.00000000000000000 ) ) ;
#14262 = FACE_OUTER_BOUND ( 'NONE', #5856, .T. ) ;
#14263 = DIRECTION ( 'NONE',  ( 0.000000000000000000, 1.000000000000000000, -1.224646799147353207E-16 ) ) ;
#14264 = ORIENTED_EDGE ( 'NONE', *, *, #9738, .F. ) ;
#14265 = DIRECTION ( 'NONE',  ( 1.156482317317883755E-15, -0.000000000000000000, 1.000000000000000000 ) ) ;
#14266 = CARTESIAN_POINT ( 'NONE',  ( 1.163414459189985485E-15, 66.00000000000000000, 9.500000000000000000 ) ) ;
#14267 = ORIENTED_EDGE ( 'NONE', *, *, #9600, .T. ) ;
#14268 = AXIS2_PLACEMENT_3D ( 'NONE', #4276, #320, #15852 ) ;
#14269 = VECTOR ( 'NONE', #3830, 1000.000000000000000 ) ;
#14270 = DIRECTION ( 'NONE',  ( 0.000000000000000000, 1.000000000000000000, 0.000000000000000000 ) ) ;
#14271 = EDGE_CURVE ( 'NONE', #214, #11801, #12103, .T. ) ;
#14272 = ORIENTED_EDGE ( 'NONE', *, *, #2311, .T. ) ;
#14273 = ORIENTED_EDGE ( 'NONE', *, *, #15469, .F. ) ;
#14274 = CYLINDRICAL_SURFACE ( 'NONE', #14658, 34.00000000000000000 ) ;
#14275 = VERTEX_POINT ( 'NONE', #2089 ) ;
#14276 = CARTESIAN_POINT ( 'NONE',  ( 0.000000000000000000, 0.000000000000000000, 0.000000000000000000 ) ) ;
#14277 = ORIENTED_EDGE ( 'NONE', *, *, #6234, .T. ) ;
#14278 = CIRCLE ( 'NONE', #2478, 7.999999999999996447 ) ;
#14279 = EDGE_LOOP ( 'NONE', ( #1489, #6440 ) ) ;
#14280 = CYLINDRICAL_SURFACE ( 'NONE', #14034, 4.006599999998781136 ) ;
#14281 = CARTESIAN_POINT ( 'NONE',  ( 45.00000000000000000, 515.4878487013597805, -546.7230258972048205 ) ) ;
#14282 = VERTEX_POINT ( 'NONE', #13774 ) ;
#14283 = DIRECTION ( 'NONE',  ( -1.000000000000000000, 0.000000000000000000, 0.000000000000000000 ) ) ;
#14284 = DIRECTION ( 'NONE',  ( 2.920976200236518919E-15, -0.9950371902099892640, -0.09950371902099772181 ) ) ;
#14285 = CARTESIAN_POINT ( 'NONE',  ( 75.00000000000000000, 0.000000000000000000, 0.000000000000000000 ) ) ;
#14286 = VERTEX_POINT ( 'NONE', #16512 ) ;
#14287 = CARTESIAN_POINT ( 'NONE',  ( -2.220446049250313081E-13, 75.00000000000001421, 3.000000000000000000 ) ) ;
#14288 = PLANE ( 'NONE',  #5286 ) ;
#14289 = ORIENTED_EDGE ( 'NONE', *, *, #5840, .F. ) ;
#14290 = AXIS2_PLACEMENT_3D ( 'NONE', #6919, #418, #16203 ) ;
#14291 = PLANE ( 'NONE',  #3312 ) ;
#14292 = ORIENTED_EDGE ( 'NONE', *, *, #12106, .T. ) ;
#14293 = PLANE ( 'NONE',  #5904 ) ;
#14294 = ORIENTED_EDGE ( 'NONE', *, *, #4255, .T. ) ;
#14295 = ORIENTED_EDGE ( 'NONE', *, *, #15310, .T. ) ;
#14296 = FACE_BOUND ( 'NONE', #14563, .T. ) ;
#14297 = FACE_OUTER_BOUND ( 'NONE', #14818, .T. ) ;
#14298 = CARTESIAN_POINT ( 'NONE',  ( 0.7365999999999761627, 261.2094592450223445, 287.2045212030221251 ) ) ;
#14299 = AXIS2_PLACEMENT_3D ( 'NONE', #4933, #5896, #4607 ) ;
#14300 = ORIENTED_EDGE ( 'NONE', *, *, #6361, .T. ) ;
#14301 = ADVANCED_FACE ( 'NONE', ( #4742 ), #5707, .T. ) ;
#14302 = DIRECTION ( 'NONE',  ( -0.000000000000000000, -1.000000000000000000, -0.000000000000000000 ) ) ;
#14303 = CARTESIAN_POINT ( 'NONE',  ( -33.00000000000000000, 8.000000000000000000, -22.00000000000000355 ) ) ;
#14304 = CARTESIAN_POINT ( 'NONE',  ( 0.000000000000000000, 66.00000000000000000, 1.799999999999999600 ) ) ;
#14305 = CLOSED_SHELL ( 'NONE', ( #16738, #10690, #2984, #2238, #14301, #6830, #4024, #3497, #13508, #11439, #10543, #16121, #3815, #14148, #12119, #1414, #1535, #15809, #10335, #10929, #11486, #2699, #15193, #16334, #14456, #577, #3734, #9824, #6334, #14152, #11078, #14328, #6754, #14355, #6734, #13131, #6330, #14879, #3736, #382, #1829, #8158, #5162, #5491 ) ) ;
#14306 = VECTOR ( 'NONE', #9690, 1000.000000000000000 ) ;
#14307 = FACE_BOUND ( 'NONE', #5364, .T. ) ;
#14308 = LINE ( 'NONE', #1085, #12679 ) ;
#14309 = ADVANCED_FACE ( 'NONE', ( #13696 ), #8535, .T. ) ;
#14310 = CARTESIAN_POINT ( 'NONE',  ( 21.99999999999998224, 6.000000000000000000, -31.99999999999998579 ) ) ;
#14311 = LINE ( 'NONE', #9253, #146 ) ;
#14313 = VERTEX_POINT ( 'NONE', #3146 ) ;
#14312 = EDGE_LOOP ( 'NONE', ( #6404, #15306 ) ) ;
#14314 = AXIS2_PLACEMENT_3D ( 'NONE', #5422, #5599, #205 ) ;
#14315 = CARTESIAN_POINT ( 'NONE',  ( 394.0000000000001137, 339.4485271457189128, -10.62862937063367852 ) ) ;
#14316 = AXIS2_PLACEMENT_3D ( 'NONE', #7762, #16874, #5448 ) ;
#14317 = PLANE ( 'NONE',  #3622 ) ;
#14318 = VECTOR ( 'NONE', #11555, 1000.000000000000000 ) ;
#14319 = VECTOR ( 'NONE', #10689, 1000.000000000000227 ) ;
#14320 = DIRECTION ( 'NONE',  ( 0.000000000000000000, 0.000000000000000000, 1.000000000000000000 ) ) ;
#14321 = ORIENTED_EDGE ( 'NONE', *, *, #4040, .T. ) ;
#14322 = EDGE_CURVE ( 'NONE', #12051, #2662, #2002, .T. ) ;
#14323 = DIRECTION ( 'NONE',  ( 0.000000000000000000, 0.000000000000000000, 1.000000000000000000 ) ) ;
#14324 = AXIS2_PLACEMENT_3D ( 'NONE', #1630, #5320, #9543 ) ;
#14325 = PLANE ( 'NONE',  #16080 ) ;
#14326 = VERTEX_POINT ( 'NONE', #5787 ) ;
#14327 = CARTESIAN_POINT ( 'NONE',  ( -46.99999999999988631, 473.6663340069157471, -545.1966447803968094 ) ) ;
#14328 = ADVANCED_FACE ( 'NONE', ( #4653 ), #639, .T. ) ;
#14329 = CYLINDRICAL_SURFACE ( 'NONE', #12307, 2.500000000000002220 ) ;
#14330 = CARTESIAN_POINT ( 'NONE',  ( 3.674999999999999822, 0.000000000000000000, 0.000000000000000000 ) ) ;
#14331 = CYLINDRICAL_SURFACE ( 'NONE', #1694, 4.999999999999997335 ) ;
#14332 = EDGE_CURVE ( 'NONE', #3447, #10304, #8381, .T. ) ;
#14333 = EDGE_CURVE ( 'NONE', #1391, #7963, #4588, .T. ) ;
#14334 = AXIS2_PLACEMENT_3D ( 'NONE', #1351, #10541, #3932 ) ;
#14335 = CARTESIAN_POINT ( 'NONE',  ( 55.99999999999989342, 523.2161522479888163, -502.8936384967199729 ) ) ;
#14336 = FACE_OUTER_BOUND ( 'NONE', #5232, .T. ) ;
#14337 = VERTEX_POINT ( 'NONE', #9758 ) ;
#14338 = CARTESIAN_POINT ( 'NONE',  ( 1.224999999999999867, 15.25000000000000000, 0.000000000000000000 ) ) ;
#14339 =( REPRESENTATION_RELATIONSHIP ('NONE','NONE', #15277, #584 ) REPRESENTATION_RELATIONSHIP_WITH_TRANSFORMATION ( #1201 )SHAPE_REPRESENTATION_RELATIONSHIP( ) );
#14340 = AXIS2_PLACEMENT_3D ( 'NONE', #11321, #5748, #16224 ) ;
#14341 = DIRECTION ( 'NONE',  ( 0.000000000000000000, 0.000000000000000000, -1.000000000000000000 ) ) ;
#14342 = STYLED_ITEM ( 'NONE', ( #5694 ), #2742 ) ;
#14343 = VERTEX_POINT ( 'NONE', #14989 ) ;
#14344 = VECTOR ( 'NONE', #11501, 1000.000000000000000 ) ;
#14345 = CIRCLE ( 'NONE', #3379, 0.5249999999999994671 ) ;
#14346 = LINE ( 'NONE', #12972, #16515 ) ;
#14347 = CARTESIAN_POINT ( 'NONE',  ( 31.00000000000000000, 19.00000000000000000, 30.99999999999999289 ) ) ;
#14348 = DIRECTION ( 'NONE',  ( 1.000000000000000000, -0.000000000000000000, 0.000000000000000000 ) ) ;
#14349 = EDGE_LOOP ( 'NONE', ( #4059, #9245, #10429, #12311 ) ) ;
#14350 = DIRECTION ( 'NONE',  ( 0.000000000000000000, 0.000000000000000000, 1.000000000000000000 ) ) ;
#14351 = EDGE_CURVE ( 'NONE', #7927, #583, #5872, .T. ) ;
#14352 = DIRECTION ( 'NONE',  ( -1.000000000000000000, 0.000000000000000000, 0.000000000000000000 ) ) ;
#14353 = ORIENTED_EDGE ( 'NONE', *, *, #16214, .T. ) ;
#14354 = EDGE_CURVE ( 'NONE', #15297, #11097, #16354, .T. ) ;
#14355 = ADVANCED_FACE ( 'NONE', ( #12487 ), #732, .F. ) ;
#14356 = FACE_OUTER_BOUND ( 'NONE', #6777, .T. ) ;
#14357 = ORIENTED_EDGE ( 'NONE', *, *, #3560, .T. ) ;
#14358 = ORIENTED_EDGE ( 'NONE', *, *, #11444, .T. ) ;
#14359 = DIRECTION ( 'NONE',  ( -0.000000000000000000, -1.000000000000000000, -0.000000000000000000 ) ) ;
#14360 = CIRCLE ( 'NONE', #6116, 9.000000000000007105 ) ;
#14361 = CIRCLE ( 'NONE', #3663, 4.695405383896011919 ) ;
#14362 = VECTOR ( 'NONE', #5531, 1000.000000000000000 ) ;
#14363 = EDGE_LOOP ( 'NONE', ( #11972, #15730, #14507, #2416 ) ) ;
#14364 = DIRECTION ( 'NONE',  ( 1.000000000000000000, 0.000000000000000000, 0.000000000000000000 ) ) ;
#14365 = ORIENTED_EDGE ( 'NONE', *, *, #11497, .F. ) ;
#14366 = CIRCLE ( 'NONE', #9985, 12.00000000000000178 ) ;
#14367 = ORIENTED_EDGE ( 'NONE', *, *, #1317, .T. ) ;
#14368 = DIRECTION ( 'NONE',  ( 0.000000000000000000, 0.000000000000000000, 1.000000000000000000 ) ) ;
#14369 = CARTESIAN_POINT ( 'NONE',  ( 35.99999999999999289, 10.00000000000000000, 17.99999999999998934 ) ) ;
#14370 = AXIS2_PLACEMENT_3D ( 'NONE', #1992, #7223, #4730 ) ;
#14371 = VERTEX_POINT ( 'NONE', #10393 ) ;
#14372 = CARTESIAN_POINT ( 'NONE',  ( 0.000000000000000000, 396.9484440344699010, -165.7668752622531088 ) ) ;
#14373 = AXIS2_PLACEMENT_3D ( 'NONE', #14622, #2682, #119 ) ;
#14374 = CARTESIAN_POINT ( 'NONE',  ( -54.99999999999999289, 515.4878487013597805, -546.7230258972048205 ) ) ;
#14375 = DIRECTION ( 'NONE',  ( 0.000000000000000000, 0.000000000000000000, -1.000000000000000000 ) ) ;
#14376 = AXIS2_PLACEMENT_3D ( 'NONE', #12332, #3061, #13788 ) ;
#14377 = LINE ( 'NONE', #7656, #5847 ) ;
#14378 = ORIENTED_EDGE ( 'NONE', *, *, #5423, .T. ) ;
#14379 = DIRECTION ( 'NONE',  ( -1.000000000000000000, -0.000000000000000000, -0.000000000000000000 ) ) ;
#14380 = DIRECTION ( 'NONE',  ( 0.000000000000000000, -0.9271838545667884235, 0.3746065934159092392 ) ) ;
#14381 = VECTOR ( 'NONE', #12614, 1000.000000000000000 ) ;
#14382 = ORIENTED_EDGE ( 'NONE', *, *, #241, .F. ) ;
#14383 = CARTESIAN_POINT ( 'NONE',  ( 10.00000000000000000, 363.9544815475646260, -322.6258333628447872 ) ) ;
#14384 = ORIENTED_EDGE ( 'NONE', *, *, #8048, .T. ) ;
#14385 = FACE_OUTER_BOUND ( 'NONE', #7642, .T. ) ;
#14386 =( GEOMETRIC_REPRESENTATION_CONTEXT ( 3 ) GLOBAL_UNCERTAINTY_ASSIGNED_CONTEXT ( ( #5482 ) ) GLOBAL_UNIT_ASSIGNED_CONTEXT ( ( #4737, #11268, #8712 ) ) REPRESENTATION_CONTEXT ( 'NONE', 'WORKASPACE' ) );
#14387 = VECTOR ( 'NONE', #7168, 1000.000000000000000 ) ;
#14388 = VERTEX_POINT ( 'NONE', #10473 ) ;
#14389 = ORIENTED_EDGE ( 'NONE', *, *, #4995, .F. ) ;
#14390 = SURFACE_SIDE_STYLE ('',( #6465 ) ) ;
#14391 = AXIS2_PLACEMENT_3D ( 'NONE', #7795, #11759, #10389 ) ;
#14392 = EDGE_CURVE ( 'NONE', #9971, #1418, #15319, .T. ) ;
#14393 = CARTESIAN_POINT ( 'NONE',  ( 31.00000000000003553, 10.00000000000000000, -22.99999999999999645 ) ) ;
#14394 = DIRECTION ( 'NONE',  ( -1.000000000000000000, -0.000000000000000000, -0.000000000000000000 ) ) ;
#14395 = EDGE_LOOP ( 'NONE', ( #15694, #3133, #3445, #2773 ) ) ;
#14396 = CARTESIAN_POINT ( 'NONE',  ( 56.73000000000001108, 239.4632308570078294, 56.73739990498292940 ) ) ;
#14397 = PRODUCT_DEFINITION_SHAPE ( 'NONE', 'NONE',  #16982 ) ;
#14398 = CARTESIAN_POINT ( 'NONE',  ( -21.00000000000002842, 0.000000000000000000, -32.49999999999999289 ) ) ;
#14399 = DIRECTION ( 'NONE',  ( -0.000000000000000000, -0.000000000000000000, 1.000000000000000000 ) ) ;
#14400 = FACE_OUTER_BOUND ( 'NONE', #2679, .T. ) ;
#14401 = FACE_OUTER_BOUND ( 'NONE', #13655, .T. ) ;
#14402 = AXIS2_PLACEMENT_3D ( 'NONE', #11841, #9536, #3000 ) ;
#14403 = CARTESIAN_POINT ( 'NONE',  ( 30.99999999999995737, 3.000000000000000000, 31.00000000000000000 ) ) ;
#14404 = FACE_OUTER_BOUND ( 'NONE', #12173, .T. ) ;
#14406 = ORIENTED_EDGE ( 'NONE', *, *, #10615, .F. ) ;
#14405 = ORIENTED_EDGE ( 'NONE', *, *, #16352, .F. ) ;
#14407 = DIRECTION ( 'NONE',  ( 0.000000000000000000, -1.850371707708599493E-15, -1.000000000000000000 ) ) ;
#14408 = EDGE_CURVE ( 'NONE', #11618, #12955, #16249, .T. ) ;
#14409 = LINE ( 'NONE', #9004, #9104 ) ;
#14410 = FACE_OUTER_BOUND ( 'NONE', #3360, .T. ) ;
#14411 = CARTESIAN_POINT ( 'NONE',  ( -49.99999999999999289, 515.4878487013597805, -631.7230258972047068 ) ) ;
#14412 = EDGE_CURVE ( 'NONE', #10374, #10263, #5399, .T. ) ;
#14413 = VERTEX_POINT ( 'NONE', #14432 ) ;
#14414 = AXIS2_PLACEMENT_3D ( 'NONE', #15529, #3767, #9003 ) ;
#14415 = CARTESIAN_POINT ( 'NONE',  ( 1.750000000000000000, -14.59999999999999964, -1.827785347727424768E-15 ) ) ;
#14416 = DIRECTION ( 'NONE',  ( 0.000000000000000000, 0.000000000000000000, 1.000000000000000000 ) ) ;
#14417 = VERTEX_POINT ( 'NONE', #3554 ) ;
#14418 = LINE ( 'NONE', #11491, #12080 ) ;
#14419 = FACE_OUTER_BOUND ( 'NONE', #16732, .T. ) ;
#14420 = EDGE_LOOP ( 'NONE', ( #11054, #12613, #11506, #13036 ) ) ;
#14421 = LINE ( 'NONE', #6767, #9691 ) ;
#14422 = CARTESIAN_POINT ( 'NONE',  ( 55.99999999999989342, 493.2350855268092573, -585.2659423243250103 ) ) ;
#14423 = CARTESIAN_POINT ( 'NONE',  ( -54.99999999999999289, 645.2345343053611941, -411.3640676610526157 ) ) ;
#14424 = ORIENTED_EDGE ( 'NONE', *, *, #9551, .T. ) ;
#14425 = VECTOR ( 'NONE', #7310, 1000.000000000000000 ) ;
#14426 = DIRECTION ( 'NONE',  ( 0.000000000000000000, 7.137148015447440312E-15, -1.000000000000000000 ) ) ;
#14427 = ADVANCED_FACE ( 'NONE', ( #14512 ), #15710, .F. ) ;
#14428 = AXIS2_PLACEMENT_3D ( 'NONE', #3487, #2188, #1154 ) ;
#14429 = ADVANCED_FACE ( 'NONE', ( #180 ), #15139, .T. ) ;
#14430 =( NAMED_UNIT ( * ) SI_UNIT ( $, .STERADIAN. ) SOLID_ANGLE_UNIT ( ) );
#14431 = EDGE_CURVE ( 'NONE', #1567, #6332, #10482, .T. ) ;
#14432 = CARTESIAN_POINT ( 'NONE',  ( 394.0000000000001137, 341.5974953295086038, -15.94751227074151956 ) ) ;
#14433 = EDGE_CURVE ( 'NONE', #15367, #15832, #3471, .T. ) ;
#14434 = ORIENTED_EDGE ( 'NONE', *, *, #13909, .F. ) ;
#14435 = EDGE_CURVE ( 'NONE', #14313, #16667, #8791, .T. ) ;
#14436 = LINE ( 'NONE', #1210, #14875 ) ;
#14437 = DIRECTION ( 'NONE',  ( 1.000000000000000000, 0.000000000000000000, -0.000000000000000000 ) ) ;
#14438 = VECTOR ( 'NONE', #946, 1000.000000000000000 ) ;
#14439 = DIRECTION ( 'NONE',  ( -3.854941057726249437E-16, 0.000000000000000000, -1.000000000000000000 ) ) ;
#14440 = ORIENTED_EDGE ( 'NONE', *, *, #9055, .T. ) ;
#14441 = VECTOR ( 'NONE', #10209, 1000.000000000000000 ) ;
#14442 = LINE ( 'NONE', #99, #16007 ) ;
#14443 = FACE_OUTER_BOUND ( 'NONE', #14695, .T. ) ;
#14444 = DIRECTION ( 'NONE',  ( 0.000000000000000000, 0.000000000000000000, 1.000000000000000000 ) ) ;
#14445 = EDGE_LOOP ( 'NONE', ( #3366, #13297, #6802, #14976 ) ) ;
#14446 = DIRECTION ( 'NONE',  ( 0.000000000000000000, 0.000000000000000000, -1.000000000000000000 ) ) ;
#14447 = EDGE_LOOP ( 'NONE', ( #9320, #7660, #5177, #10338 ) ) ;
#14448 = VERTEX_POINT ( 'NONE', #1458 ) ;
#14449 = LINE ( 'NONE', #13156, #956 ) ;
#14450 = ADVANCED_FACE ( 'NONE', ( #11363 ), #6505, .F. ) ;
#14451 = ORIENTED_EDGE ( 'NONE', *, *, #6753, .F. ) ;
#14452 = ORIENTED_EDGE ( 'NONE', *, *, #7002, .F. ) ;
#14453 = CARTESIAN_POINT ( 'NONE',  ( 0.000000000000000000, 0.000000000000000000, 0.000000000000000000 ) ) ;
#14454 = VECTOR ( 'NONE', #1778, 1000.000000000000000 ) ;
#14455 = EDGE_LOOP ( 'NONE', ( #9573, #4805 ) ) ;
#14456 = ADVANCED_FACE ( 'NONE', ( #6420 ), #2575, .F. ) ;
#14457 = ADVANCED_FACE ( 'NONE', ( #2170 ), #4834, .T. ) ;
#14458 = ADVANCED_FACE ( 'NONE', ( #12651, #6587, #91 ), #16904, .T. ) ;
#14459 = ORIENTED_EDGE ( 'NONE', *, *, #4733, .T. ) ;
#14460 = EDGE_CURVE ( 'NONE', #13400, #1978, #8010, .T. ) ;
#14461 = LINE ( 'NONE', #2503, #1702 ) ;
#14462 = FACE_OUTER_BOUND ( 'NONE', #7683, .T. ) ;
#14463 = VERTEX_POINT ( 'NONE', #11845 ) ;
#14464 = DIRECTION ( 'NONE',  ( -0.000000000000000000, -0.000000000000000000, 1.000000000000000000 ) ) ;
#14465 = DIRECTION ( 'NONE',  ( -1.000000000000000000, -0.000000000000000000, -0.000000000000000000 ) ) ;
#14466 = AXIS2_PLACEMENT_3D ( 'NONE', #9571, #8104, #2864 ) ;
#14467 = PLANE ( 'NONE',  #7753 ) ;
#14468 = ORIENTED_EDGE ( 'NONE', *, *, #14545, .F. ) ;
#14469 = CARTESIAN_POINT ( 'NONE',  ( 10.00000000000000000, 372.8685141053783241, -150.1198051533980049 ) ) ;
#14470 = CARTESIAN_POINT ( 'NONE',  ( 0.000000000000000000, 309.2289037985890445, -150.1198051533984597 ) ) ;
#14471 = ORIENTED_EDGE ( 'NONE', *, *, #14126, .F. ) ;
#14472 = DIRECTION ( 'NONE',  ( -1.000000000000000000, -0.000000000000000000, -0.000000000000000000 ) ) ;
#14473 = ORIENTED_EDGE ( 'NONE', *, *, #10841, .F. ) ;
#14474 = CARTESIAN_POINT ( 'NONE',  ( 0.000000000000000000, 10.00000000000000000, 0.000000000000000000 ) ) ;
#14475 = VERTEX_POINT ( 'NONE', #5317 ) ;
#14476 = CIRCLE ( 'NONE', #10355, 20.75209553982837463 ) ;
#14477 = ORIENTED_EDGE ( 'NONE', *, *, #587, .T. ) ;
#14478 = FACE_OUTER_BOUND ( 'NONE', #3782, .T. ) ;
#14479 = EDGE_CURVE ( 'NONE', #4138, #9177, #6111, .T. ) ;
#14480 = MANIFOLD_SOLID_BREP ( 'Boss-Extrude4', #15671 ) ;
#14481 = LINE ( 'NONE', #14222, #6591 ) ;
#14482 = CARTESIAN_POINT ( 'NONE',  ( -46.99999999999988631, 493.2350855268086320, -494.4847040861889127 ) ) ;
#14483 = ORIENTED_EDGE ( 'NONE', *, *, #1523, .T. ) ;
#14484 = CARTESIAN_POINT ( 'NONE',  ( 30.99999999999999645, 0.000000000000000000, -25.99999999999999645 ) ) ;
#14485 = DIRECTION ( 'NONE',  ( -0.000000000000000000, -1.000000000000000000, -0.000000000000000000 ) ) ;
#14486 = DIRECTION ( 'NONE',  ( 1.000000000000000000, 0.000000000000000000, 0.000000000000000000 ) ) ;
#14487 = CARTESIAN_POINT ( 'NONE',  ( 56.73000000000001108, 239.4632308570078294, 86.73739990498292229 ) ) ;
#14488 = DIRECTION ( 'NONE',  ( 0.000000000000000000, 1.000000000000000000, 0.000000000000000000 ) ) ;
#14489 = FACE_OUTER_BOUND ( 'NONE', #1113, .T. ) ;
#14490 = VECTOR ( 'NONE', #4266, 1000.000000000000000 ) ;
#14491 = DIRECTION ( 'NONE',  ( 0.000000000000000000, -1.000000000000000000, 0.000000000000000000 ) ) ;
#14492 = ADVANCED_FACE ( 'NONE', ( #13326 ), #14066, .T. ) ;
#14494 = VERTEX_POINT ( 'NONE', #12024 ) ;
#14493 = ORIENTED_EDGE ( 'NONE', *, *, #11891, .T. ) ;
#14495 = DIRECTION ( 'NONE',  ( 0.000000000000000000, 0.000000000000000000, -1.000000000000000000 ) ) ;
#14496 = ADVANCED_FACE ( 'NONE', ( #4116 ), #7105, .T. ) ;
#14497 = CARTESIAN_POINT ( 'NONE',  ( 0.3042215205874465589, 286.0197353374350655, 37.35332311086187929 ) ) ;
#14498 = DIRECTION ( 'NONE',  ( -0.000000000000000000, -1.000000000000000000, 0.000000000000000000 ) ) ;
#14499 = PLANE ( 'NONE',  #8027 ) ;
#14500 = ORIENTED_EDGE ( 'NONE', *, *, #3760, .F. ) ;
#14501 = AXIS2_PLACEMENT_3D ( 'NONE', #8124, #14909, #8390 ) ;
#14502 = CARTESIAN_POINT ( 'NONE',  ( 30.99999999999997513, 10.00000000000000000, 30.99999999999999645 ) ) ;
#14503 = DIRECTION ( 'NONE',  ( 0.000000000000000000, -0.6427876096865404731, 0.7660444431189771253 ) ) ;
#14504 = ORIENTED_EDGE ( 'NONE', *, *, #16113, .F. ) ;
#14505 = LINE ( 'NONE', #11928, #16720 ) ;
#14506 = CARTESIAN_POINT ( 'NONE',  ( 0.000000000000000000, 26.00000000000000000, -36.50000000000000000 ) ) ;
#14507 = ORIENTED_EDGE ( 'NONE', *, *, #2051, .F. ) ;
#14508 = DIRECTION ( 'NONE',  ( 0.000000000000000000, 0.000000000000000000, 1.000000000000000000 ) ) ;
#14509 = CARTESIAN_POINT ( 'NONE',  ( -46.99999999999988631, 493.2350855268086320, -512.8755148539809170 ) ) ;
#14510 = ORIENTED_EDGE ( 'NONE', *, *, #10742, .F. ) ;
#14511 = LINE ( 'NONE', #15792, #5892 ) ;
#14512 = FACE_OUTER_BOUND ( 'NONE', #2934, .T. ) ;
#14513 = CIRCLE ( 'NONE', #1381, 36.50000000000000000 ) ;
#14514 = EDGE_LOOP ( 'NONE', ( #14500, #12937, #7125, #13494 ) ) ;
#14515 = DIRECTION ( 'NONE',  ( 0.000000000000000000, 0.000000000000000000, -1.000000000000000000 ) ) ;
#14516 = CARTESIAN_POINT ( 'NONE',  ( 0.000000000000000000, 10.00000000000000000, 0.000000000000000000 ) ) ;
#14517 = EDGE_CURVE ( 'NONE', #11329, #1995, #11315, .T. ) ;
#14518 = DIRECTION ( 'NONE',  ( -1.000000000000000000, 0.000000000000000000, 0.000000000000000000 ) ) ;
#14519 = ORIENTED_EDGE ( 'NONE', *, *, #7918, .F. ) ;
#14520 = LINE ( 'NONE', #1637, #9430 ) ;
#14521 = CARTESIAN_POINT ( 'NONE',  ( 0.7366000000000268999, 217.7170024689957302, 287.2045212030222388 ) ) ;
#14522 = DIRECTION ( 'NONE',  ( 0.000000000000000000, -1.000000000000000000, 0.000000000000000000 ) ) ;
#14523 = VERTEX_POINT ( 'NONE', #9451 ) ;
#14524 = ORIENTED_EDGE ( 'NONE', *, *, #8561, .F. ) ;
#14525 = ORIENTED_EDGE ( 'NONE', *, *, #10040, .F. ) ;
#14526 = EDGE_CURVE ( 'NONE', #12218, #15841, #602, .T. ) ;
#14527 = AXIS2_PLACEMENT_3D ( 'NONE', #5663, #14855, #11942 ) ;
#14528 = LINE ( 'NONE', #5417, #11095 ) ;
#14529 = VERTEX_POINT ( 'NONE', #2829 ) ;
#14530 = SHAPE_DEFINITION_REPRESENTATION ( #15341, #15277 ) ;
#14531 = PRODUCT_DEFINITION_SHAPE ( 'NONE', 'NONE',  #16984 ) ;
#14532 = VERTEX_POINT ( 'NONE', #10644 ) ;
#14533 = ORIENTED_EDGE ( 'NONE', *, *, #8022, .T. ) ;
#14534 = DIRECTION ( 'NONE',  ( -1.000000000000000000, 0.000000000000000000, 0.000000000000000000 ) ) ;
#14535 = DIRECTION ( 'NONE',  ( -0.000000000000000000, -1.000000000000000000, -0.000000000000000000 ) ) ;
#14536 = VECTOR ( 'NONE', #13465, 1000.000000000000000 ) ;
#14537 = EDGE_CURVE ( 'NONE', #12698, #7827, #4386, .T. ) ;
#14538 = ORIENTED_EDGE ( 'NONE', *, *, #14710, .T. ) ;
#14540 = LINE ( 'NONE', #10591, #1182 ) ;
#14539 = AXIS2_PLACEMENT_3D ( 'NONE', #6301, #3584, #1009 ) ;
#14541 = CARTESIAN_POINT ( 'NONE',  ( -39.99999999999997868, 0.000000000000000000, -25.99999999999999645 ) ) ;
#14542 = VERTEX_POINT ( 'NONE', #14857 ) ;
#14543 = STYLED_ITEM ( 'NONE', ( #11421 ), #3183 ) ;
#14544 = CARTESIAN_POINT ( 'NONE',  ( 30.99999999999997158, 0.000000000000000000, 19.99999999999999289 ) ) ;
#14545 = EDGE_CURVE ( 'NONE', #12295, #4162, #345, .T. ) ;
#14546 = VERTEX_POINT ( 'NONE', #4460 ) ;
#14547 = CARTESIAN_POINT ( 'NONE',  ( 435.7731165870194445, 329.6061121441327941, 0.000000000000000000 ) ) ;
#14548 = DIRECTION ( 'NONE',  ( 0.000000000000000000, 0.000000000000000000, 1.000000000000000000 ) ) ;
#14549 = VERTEX_POINT ( 'NONE', #7026 ) ;
#14550 = EDGE_CURVE ( 'NONE', #2782, #14286, #10992, .T. ) ;
#14551 = EDGE_CURVE ( 'NONE', #5917, #16466, #7459, .T. ) ;
#14552 = EDGE_CURVE ( 'NONE', #11763, #3738, #8326, .T. ) ;
#14553 = CARTESIAN_POINT ( 'NONE',  ( -46.99999999999988631, 523.2161522479893847, -576.8570079137933817 ) ) ;
#14554 = VERTEX_POINT ( 'NONE', #10823 ) ;
#14555 = CARTESIAN_POINT ( 'NONE',  ( 1.163414457778310218E-15, 63.00000000000000000, 9.500000000000000000 ) ) ;
#14556 = AXIS2_PLACEMENT_3D ( 'NONE', #14136, #2270, #5100 ) ;
#14557 = AXIS2_PLACEMENT_3D ( 'NONE', #16024, #1598, #7854 ) ;
#14558 = ORIENTED_EDGE ( 'NONE', *, *, #8643, .T. ) ;
#14559 = EDGE_LOOP ( 'NONE', ( #13679, #5340, #13069, #137 ) ) ;
#14560 = FACE_OUTER_BOUND ( 'NONE', #10835, .T. ) ;
#14561 = CYLINDRICAL_SURFACE ( 'NONE', #13754, 13.69540538389601991 ) ;
#14562 = DIRECTION ( 'NONE',  ( 0.000000000000000000, 0.000000000000000000, -1.000000000000000000 ) ) ;
#14563 = EDGE_LOOP ( 'NONE', ( #8724, #4875 ) ) ;
#14564 = CARTESIAN_POINT ( 'NONE',  ( 36.99999999999999289, 0.000000000000000000, 22.99999999999999645 ) ) ;
#14565 = CYLINDRICAL_SURFACE ( 'NONE', #12435, 2.500000000000002220 ) ;
#14566 = CIRCLE ( 'NONE', #5783, 20.75209553982837463 ) ;
#14567 = CARTESIAN_POINT ( 'NONE',  ( -46.99999999999988631, 523.2161522479888163, -507.5890438806159750 ) ) ;
#14568 = ADVANCED_FACE ( 'NONE', ( #8067 ), #4304, .T. ) ;
#14569 = DIRECTION ( 'NONE',  ( -1.000000000000000000, -0.000000000000000000, 0.000000000000000000 ) ) ;
#14570 = FACE_OUTER_BOUND ( 'NONE', #12292, .T. ) ;
#14571 = EDGE_CURVE ( 'NONE', #2235, #4006, #11159, .T. ) ;
#14572 = CARTESIAN_POINT ( 'NONE',  ( -8.632284108936165032E-13, 289.4632308570086252, 37.52989836422091230 ) ) ;
#14574 = ORIENTED_EDGE ( 'NONE', *, *, #5099, .T. ) ;
#14573 = EDGE_LOOP ( 'NONE', ( #5988, #8229, #7538, #3908 ) ) ;
#14575 = CARTESIAN_POINT ( 'NONE',  ( 19.99999999999995381, 3.000000000000000000, -36.99999999999999289 ) ) ;
#14576 = CIRCLE ( 'NONE', #11280, 3.300000000000011369 ) ;
#14577 = CARTESIAN_POINT ( 'NONE',  ( -3.269999999998713491, 285.4366476906446906, 37.52989836422034386 ) ) ;
#14578 = CARTESIAN_POINT ( 'NONE',  ( 2.265596578422603396E-15, 19.00100000000000122, 18.50000000000000000 ) ) ;
#14579 = CARTESIAN_POINT ( 'NONE',  ( 25.99999999999996092, 3.000000000000000000, 40.00000000000000711 ) ) ;
#14580 = ORIENTED_EDGE ( 'NONE', *, *, #6625, .T. ) ;
#14581 = VECTOR ( 'NONE', #764, 1000.000000000000000 ) ;
#14582 = DIRECTION ( 'NONE',  ( 1.000000000000000000, 0.000000000000000000, 0.000000000000000000 ) ) ;
#14583 = EDGE_CURVE ( 'NONE', #3282, #4422, #12786, .T. ) ;
#14584 = CARTESIAN_POINT ( 'NONE',  ( -45.00000000000000000, 549.5810598491746077, -518.1154249974242703 ) ) ;
#14585 = VERTEX_POINT ( 'NONE', #15356 ) ;
#14586 = CARTESIAN_POINT ( 'NONE',  ( 4.549999999999999822, 1.748183305782846567E-15, 14.27500000000000036 ) ) ;
#14587 = MANIFOLD_SOLID_BREP ( 'Boss-Extrude4', #7435 ) ;
#14588 = DIRECTION ( 'NONE',  ( 0.000000000000000000, 1.000000000000000000, 0.000000000000000000 ) ) ;
#14589 = FACE_BOUND ( 'NONE', #16596, .T. ) ;
#14590 = VECTOR ( 'NONE', #16852, 1000.000000000000000 ) ;
#14591 = CARTESIAN_POINT ( 'NONE',  ( -26.00000000000002842, 0.000000000000000000, -31.00000000000003197 ) ) ;
#14592 = FACE_OUTER_BOUND ( 'NONE', #1175, .T. ) ;
#14593 = ORIENTED_EDGE ( 'NONE', *, *, #5790, .F. ) ;
#14594 = VECTOR ( 'NONE', #14302, 1000.000000000000000 ) ;
#14595 = DIRECTION ( 'NONE',  ( 0.000000000000000000, 0.000000000000000000, 1.000000000000000000 ) ) ;
#14596 = LINE ( 'NONE', #6685, #6006 ) ;
#14597 = DIRECTION ( 'NONE',  ( 0.000000000000000000, 0.000000000000000000, -1.000000000000000000 ) ) ;
#14598 = ORIENTED_EDGE ( 'NONE', *, *, #1726, .T. ) ;
#14599 = CARTESIAN_POINT ( 'NONE',  ( -31.00000000000002842, 3.000000000000000000, 31.00000000000000000 ) ) ;
#14600 = UNCERTAINTY_MEASURE_WITH_UNIT (LENGTH_MEASURE( 1.000000000000000082E-05 ), #955, 'distance_accuracy_value', 'NONE');
#14601 = CARTESIAN_POINT ( 'NONE',  ( 1.250085104875786612E-12, 220.0768326692952996, 286.9685381829922903 ) ) ;
#14602 = LINE ( 'NONE', #13415, #11409 ) ;
#14603 = EDGE_LOOP ( 'NONE', ( #13161, #5466, #8430, #2438 ) ) ;
#14604 = CARTESIAN_POINT ( 'NONE',  ( -31.00000000000003197, 19.00000000000000000, -26.00000000000000355 ) ) ;
#14605 = VECTOR ( 'NONE', #5093, 1000.000000000000000 ) ;
#14606 = VECTOR ( 'NONE', #14597, 1000.000000000000000 ) ;
#14607 = DIRECTION ( 'NONE',  ( 0.000000000000000000, 1.000000000000000000, 1.321694076934710402E-16 ) ) ;
#14608 = CYLINDRICAL_SURFACE ( 'NONE', #6455, 5.000000000000000888 ) ;
#14609 = ORIENTED_EDGE ( 'NONE', *, *, #11915, .T. ) ;
#14610 = ORIENTED_EDGE ( 'NONE', *, *, #8214, .F. ) ;
#14611 = ORIENTED_EDGE ( 'NONE', *, *, #5075, .F. ) ;
#14612 = CIRCLE ( 'NONE', #7737, 13.69540538389601991 ) ;
#14613 = LINE ( 'NONE', #13503, #10550 ) ;
#14614 = VERTEX_POINT ( 'NONE', #2128 ) ;
#14615 = APPLICATION_PROTOCOL_DEFINITION ( 'draft international standard', 'automotive_design', 1998, #15549 ) ;
#14616 = ADVANCED_FACE ( 'NONE', ( #8751 ), #11072, .F. ) ;
#14617 = CIRCLE ( 'NONE', #354, 59.99999999999994316 ) ;
#14618 = STYLED_ITEM ( 'NONE', ( #14068 ), #14587 ) ;
#14619 = EDGE_LOOP ( 'NONE', ( #7530, #12762, #13265, #9850 ) ) ;
#14620 = ORIENTED_EDGE ( 'NONE', *, *, #14130, .T. ) ;
#14621 = CYLINDRICAL_SURFACE ( 'NONE', #7432, 6.473200000000000287 ) ;
#14622 = CARTESIAN_POINT ( 'NONE',  ( -31.00000000000000000, 19.00000000000000000, 30.99999999999999289 ) ) ;
#14623 = TOROIDAL_SURFACE ( 'NONE', #10789, 14.76997474683060041, 0.5250000000000000222 ) ;
#14624 = EDGE_CURVE ( 'NONE', #5349, #11960, #5915, .T. ) ;
#14625 = ORIENTED_EDGE ( 'NONE', *, *, #2667, .T. ) ;
#14626 = LINE ( 'NONE', #15994, #4478 ) ;
#14627 = CARTESIAN_POINT ( 'NONE',  ( 45.00000000000000000, 549.5810598491746077, -518.1154249974242703 ) ) ;
#14628 = VERTEX_POINT ( 'NONE', #4795 ) ;
#14629 = CIRCLE ( 'NONE', #13539, 6.473199999999998511 ) ;
#14630 = CIRCLE ( 'NONE', #12989, 12.00000000000000000 ) ;
#14631 = VECTOR ( 'NONE', #16861, 1000.000000000000000 ) ;
#14632 = CARTESIAN_POINT ( 'NONE',  ( 0.000000000000000000, 6.452029775889750974E-16, 5.268482129199949959 ) ) ;
#14633 = AXIS2_PLACEMENT_3D ( 'NONE', #8216, #10801, #4284 ) ;
#14634 = ORIENTED_EDGE ( 'NONE', *, *, #2728, .T. ) ;
#14635 = CARTESIAN_POINT ( 'NONE',  ( 1.231978928595278688E-12, 193.4499468633042625, 37.13122676359134999 ) ) ;
#14636 = CARTESIAN_POINT ( 'NONE',  ( 32.99999999999998579, 10.00000000000000000, 21.99999999999999645 ) ) ;
#14637 = ORIENTED_EDGE ( 'NONE', *, *, #4556, .F. ) ;
#14638 = DIRECTION ( 'NONE',  ( -1.000000000000000000, 0.000000000000000000, 0.000000000000000000 ) ) ;
#14639 = ORIENTED_EDGE ( 'NONE', *, *, #10531, .F. ) ;
#14640 =( NAMED_UNIT ( * ) PLANE_ANGLE_UNIT ( ) SI_UNIT ( $, .RADIAN. ) );
#14641 = CIRCLE ( 'NONE', #653, 13.69540538389596485 ) ;
#14642 = DIRECTION ( 'NONE',  ( 0.000000000000000000, 0.000000000000000000, 1.000000000000000000 ) ) ;
#14643 = EDGE_CURVE ( 'NONE', #11379, #7379, #6641, .T. ) ;
#14644 = EDGE_CURVE ( 'NONE', #2707, #15120, #4623, .T. ) ;
#14645 = ORIENTED_EDGE ( 'NONE', *, *, #5598, .T. ) ;
#14646 = B_SPLINE_CURVE_WITH_KNOTS ( 'NONE', 3,
 ( #10705, #16036, #10537, #13468, #4604, #5641, #10964, #5891, #12420, #497, #16200, #8647, #8398, #14835, #16371, #7337 ),
 .UNSPECIFIED., .F., .F.,
 ( 4, 2, 2, 2, 2, 2, 2, 4 ),
 ( 0.000000000000000000, 0.0005901654530283999755, 0.001180330906056799951, 0.001770496359085199818, 0.002360661812113599902, 0.003540992718170399636, 0.004131158171198803623, 0.004721323624227206743 ),
 .UNSPECIFIED. ) ;
#14647 = VECTOR ( 'NONE', #15722, 1000.000000000000000 ) ;
#14648 = ORIENTED_EDGE ( 'NONE', *, *, #14526, .T. ) ;
#14649 = DIRECTION ( 'NONE',  ( 1.000000000000000000, 0.000000000000000000, -0.000000000000000000 ) ) ;
#14650 = AXIS2_PLACEMENT_3D ( 'NONE', #2421, #3807, #6445 ) ;
#14651 = DIRECTION ( 'NONE',  ( 0.000000000000000000, 0.000000000000000000, 1.000000000000000000 ) ) ;
#14652 = ADVANCED_FACE ( 'NONE', ( #10120 ), #6364, .T. ) ;
#14653 = CARTESIAN_POINT ( 'NONE',  ( 22.99999999999999289, 68.00000000000000000, 37.00000000000002132 ) ) ;
#14655 = ORIENTED_EDGE ( 'NONE', *, *, #12129, .T. ) ;
#14654 = EDGE_CURVE ( 'NONE', #11956, #9226, #11235, .T. ) ;
#14657 = ADVANCED_FACE ( 'NONE', ( #10043 ), #9871, .F. ) ;
#14656 = CYLINDRICAL_SURFACE ( 'NONE', #14316, 4.999999999999997335 ) ;
#14658 = AXIS2_PLACEMENT_3D ( 'NONE', #4986, #3879, #2495 ) ;
#14659 = CARTESIAN_POINT ( 'NONE',  ( 40.00000000000000711, 8.000000000000000000, 34.99999999999997868 ) ) ;
#14660 = AXIS2_PLACEMENT_3D ( 'NONE', #5995, #15030, #8591 ) ;
#14661 = CARTESIAN_POINT ( 'NONE',  ( -46.99999999999988631, 493.2350855268086320, -521.8755148539809170 ) ) ;
#14662 = CARTESIAN_POINT ( 'NONE',  ( -55.99999999999989342, 473.6663340069158039, -548.2494070140132862 ) ) ;
#14663 = CARTESIAN_POINT ( 'NONE',  ( 2.204364238465236069E-16, 66.00000000000000000, -1.800000000000000711 ) ) ;
#14664 = CARTESIAN_POINT ( 'NONE',  ( 394.0000000000001137, 339.3157724647196005, -10.68226574335978718 ) ) ;
#14665 = PRODUCT_DEFINITION_FORMATION_WITH_SPECIFIED_SOURCE ( 'ANY', '', #440, .NOT_KNOWN. ) ;
#14666 = DIRECTION ( 'NONE',  ( 0.000000000000000000, 0.000000000000000000, 1.000000000000000000 ) ) ;
#14667 = VECTOR ( 'NONE', #9385, 1000.000000000000000 ) ;
#14668 = LINE ( 'NONE', #4359, #11784 ) ;
#14670 = ORIENTED_EDGE ( 'NONE', *, *, #5798, .T. ) ;
#14669 = ORIENTED_EDGE ( 'NONE', *, *, #12048, .T. ) ;
#14671 = LINE ( 'NONE', #2804, #7001 ) ;
#14672 = CARTESIAN_POINT ( 'NONE',  ( 0.1739760006939537473, 285.8834916746054660, 37.40680846401821213 ) ) ;
#14673 = CARTESIAN_POINT ( 'NONE',  ( -54.99999999999999289, 515.4878487013597805, -631.7230258972047068 ) ) ;
#14674 = EDGE_CURVE ( 'NONE', #4133, #10494, #11318, .T. ) ;
#14675 = DIRECTION ( 'NONE',  ( 1.000000000000000000, 0.000000000000000000, -3.854941057726247958E-16 ) ) ;
#14676 = ADVANCED_FACE ( 'NONE', ( #12529 ), #16558, .F. ) ;
#14677 = ORIENTED_EDGE ( 'NONE', *, *, #8213, .F. ) ;
#14678 = PRODUCT_DEFINITION_FORMATION_WITH_SPECIFIED_SOURCE ( 'ANY', '', #1080, .NOT_KNOWN. ) ;
#14679 = EDGE_CURVE ( 'NONE', #12411, #13599, #2261, .T. ) ;
#14680 = AXIS2_PLACEMENT_3D ( 'NONE', #14347, #8163, #13414 ) ;
#14681 = DIRECTION ( 'NONE',  ( 0.000000000000000000, 0.000000000000000000, -1.000000000000000000 ) ) ;
#14682 = CARTESIAN_POINT ( 'NONE',  ( 17.00000000000000711, 380.0000000000000000, -29.71049682360898814 ) ) ;
#14683 = ORIENTED_EDGE ( 'NONE', *, *, #1019, .T. ) ;
#14684 = CARTESIAN_POINT ( 'NONE',  ( 1.050000000000000044, 0.000000000000000000, 0.000000000000000000 ) ) ;
#14685 = AXIS2_PLACEMENT_3D ( 'NONE', #9868, #7103, #15098 ) ;
#14686 = DIRECTION ( 'NONE',  ( -0.000000000000000000, -1.000000000000000000, -0.000000000000000000 ) ) ;
#14687 = DIRECTION ( 'NONE',  ( 1.000000000000000000, -0.000000000000000000, -0.000000000000000000 ) ) ;
#14688 = DIRECTION ( 'NONE',  ( 1.000000000000000000, 0.000000000000000000, -0.000000000000000000 ) ) ;
#14689 = DIRECTION ( 'NONE',  ( 0.000000000000000000, 0.000000000000000000, -1.000000000000000000 ) ) ;
#14690 = ORIENTED_EDGE ( 'NONE', *, *, #14219, .T. ) ;
#14691 = DIRECTION ( 'NONE',  ( 1.000000000000000000, -0.000000000000000000, 0.000000000000000000 ) ) ;
#14692 = DIRECTION ( 'NONE',  ( 0.000000000000000000, 0.000000000000000000, 1.000000000000000000 ) ) ;
#14693 = TOROIDAL_SURFACE ( 'NONE', #7265, 14.76997474683060041, 0.5250000000000000222 ) ;
#14694 = PRESENTATION_STYLE_ASSIGNMENT (( #10910 ) ) ;
#14695 = EDGE_LOOP ( 'NONE', ( #5141, #1522, #16197, #9422 ) ) ;
#14696 = CYLINDRICAL_SURFACE ( 'NONE', #10474, 13.69540538389596485 ) ;
#14697 = DIRECTION ( 'NONE',  ( 0.000000000000000000, 0.000000000000000000, 1.000000000000000000 ) ) ;
#14698 = ORIENTED_EDGE ( 'NONE', *, *, #10570, .F. ) ;
#14699 = DIRECTION ( 'NONE',  ( 1.000000000000000000, -0.000000000000000000, 0.000000000000000000 ) ) ;
#14700 = PLANE ( 'NONE',  #15038 ) ;
#14701 = DIRECTION ( 'NONE',  ( 1.000000000000000000, 0.000000000000000000, 0.000000000000000000 ) ) ;
#14702 = ORIENTED_EDGE ( 'NONE', *, *, #15607, .F. ) ;
#14703 = VECTOR ( 'NONE', #1216, 1000.000000000000000 ) ;
#14704 = CIRCLE ( 'NONE', #9782, 12.00000000000000178 ) ;
#14705 = FILL_AREA_STYLE ('',( #1642 ) ) ;
#14706 = EDGE_LOOP ( 'NONE', ( #4073, #9897, #14001, #8139 ) ) ;
#14707 = ORIENTED_EDGE ( 'NONE', *, *, #13739, .T. ) ;
#14708 = CARTESIAN_POINT ( 'NONE',  ( 22.99999999999995737, 0.000000000000000000, -33.99999999999998579 ) ) ;
#14709 = ORIENTED_EDGE ( 'NONE', *, *, #16630, .T. ) ;
#14710 = EDGE_CURVE ( 'NONE', #6368, #15, #13250, .T. ) ;
#14711 = DIRECTION ( 'NONE',  ( 1.000000000000000000, 0.000000000000000000, 0.000000000000000000 ) ) ;
#14712 = ORIENTED_EDGE ( 'NONE', *, *, #2697, .F. ) ;
#14713 = AXIS2_PLACEMENT_3D ( 'NONE', #10977, #5389, #6837 ) ;
#14714 = ADVANCED_FACE ( 'NONE', ( #10296 ), #1722, .T. ) ;
#14715 = ORIENTED_EDGE ( 'NONE', *, *, #11927, .T. ) ;
#14716 = CIRCLE ( 'NONE', #11965, 3.300000000000011369 ) ;
#14717 = PLANE ( 'NONE',  #16766 ) ;
#14718 = CYLINDRICAL_SURFACE ( 'NONE', #14373, 4.999999999999997335 ) ;
#14719 = VERTEX_POINT ( 'NONE', #2550 ) ;
#14720 = DIRECTION ( 'NONE',  ( 0.000000000000000000, 0.000000000000000000, -1.000000000000000000 ) ) ;
#14721 = DIRECTION ( 'NONE',  ( -1.000000000000000000, 0.000000000000000000, 0.000000000000000000 ) ) ;
#14722 = VERTEX_POINT ( 'NONE', #10205 ) ;
#14723 = PRODUCT_RELATED_PRODUCT_CATEGORY ( 'part', '', ( #14966 ) ) ;
#14724 = DIRECTION ( 'NONE',  ( 1.000000000000000000, 0.000000000000000000, 0.000000000000000000 ) ) ;
#14725 = ORIENTED_EDGE ( 'NONE', *, *, #7204, .T. ) ;
#14726 = CARTESIAN_POINT ( 'NONE',  ( -39.99999999999997868, 0.000000000000000000, 26.00000000000000355 ) ) ;
#14727 = DIRECTION ( 'NONE',  ( -0.000000000000000000, 0.000000000000000000, -1.000000000000000000 ) ) ;
#14728 = ORIENTED_EDGE ( 'NONE', *, *, #696, .T. ) ;
#14729 = AXIS2_PLACEMENT_3D ( 'NONE', #13546, #7940, #9417 ) ;
#14730 = VECTOR ( 'NONE', #16458, 1000.000000000000000 ) ;
#14731 = CARTESIAN_POINT ( 'NONE',  ( -7.877607930108291241E-13, 264.4632308570089663, 287.5298983642207986 ) ) ;
#14732 = ORIENTED_EDGE ( 'NONE', *, *, #3236, .T. ) ;
#14733 = EDGE_CURVE ( 'NONE', #9305, #9092, #15440, .T. ) ;
#14734 = CARTESIAN_POINT ( 'NONE',  ( 10.00000000000000000, 481.5601199098531993, -512.1772732904406666 ) ) ;
#14735 = ORIENTED_EDGE ( 'NONE', *, *, #4546, .F. ) ;
#14736 = ORIENTED_EDGE ( 'NONE', *, *, #3971, .F. ) ;
#14737 = LINE ( 'NONE', #5262, #3088 ) ;
#14738 = CARTESIAN_POINT ( 'NONE',  ( -18.00000000000001421, 6.000000000000000000, 36.00000000000000711 ) ) ;
#14739 = FACE_BOUND ( 'NONE', #14803, .T. ) ;
#14740 = AXIS2_PLACEMENT_3D ( 'NONE', #9681, #3155, #13872 ) ;
#14741 = AXIS2_PLACEMENT_3D ( 'NONE', #4242, #13437, #1660 ) ;
#14742 = CYLINDRICAL_SURFACE ( 'NONE', #12842, 187.4999999999998863 ) ;
#14743 = FACE_OUTER_BOUND ( 'NONE', #1833, .T. ) ;
#14744 = EDGE_CURVE ( 'NONE', #12540, #15724, #7869, .T. ) ;
#14745 = CARTESIAN_POINT ( 'NONE',  ( 394.0000000000001137, 339.1725919290084335, -110.6822657433597925 ) ) ;
#14746 = DIRECTION ( 'NONE',  ( 0.000000000000000000, 0.000000000000000000, -1.000000000000000000 ) ) ;
#14747 = EDGE_CURVE ( 'NONE', #13660, #394, #4023, .T. ) ;
#14748 = LINE ( 'NONE', #14487, #4841 ) ;
#14749 = DIRECTION ( 'NONE',  ( -0.000000000000000000, 1.000000000000000000, -0.000000000000000000 ) ) ;
#14750 = CARTESIAN_POINT ( 'NONE',  ( 39.72345254347677468, 303.2115381654813859, -6.736600000000000144 ) ) ;
#14751 = DIRECTION ( 'NONE',  ( -1.000000000000000000, 0.000000000000000000, -0.000000000000000000 ) ) ;
#14753 = ORIENTED_EDGE ( 'NONE', *, *, #615, .F. ) ;
#14752 = VERTEX_POINT ( 'NONE', #3683 ) ;
#14754 = VECTOR ( 'NONE', #11500, 1000.000000000000000 ) ;
#14755 = EDGE_CURVE ( 'NONE', #8177, #13076, #6092, .T. ) ;
#14756 = DIRECTION ( 'NONE',  ( 0.000000000000000000, 0.000000000000000000, -1.000000000000000000 ) ) ;
#14757 = CARTESIAN_POINT ( 'NONE',  ( -0.3121190734747821827, 289.3528227838037878, 37.58596727633977963 ) ) ;
#14758 = CARTESIAN_POINT ( 'NONE',  ( 56.72999999999999687, 264.4632308570091368, 287.5298983642207986 ) ) ;
#14759 = FACE_OUTER_BOUND ( 'NONE', #4731, .T. ) ;
#14760 = ORIENTED_EDGE ( 'NONE', *, *, #8927, .F. ) ;
#14761 = DIRECTION ( 'NONE',  ( 0.000000000000000000, 0.000000000000000000, -1.000000000000000000 ) ) ;
#14762 = VECTOR ( 'NONE', #11230, 1000.000000000000000 ) ;
#14763 = DIRECTION ( 'NONE',  ( 0.000000000000000000, 0.000000000000000000, -1.000000000000000000 ) ) ;
#14765 = ADVANCED_FACE ( 'NONE', ( #13124 ), #14499, .F. ) ;
#14764 = ORIENTED_EDGE ( 'NONE', *, *, #4256, .T. ) ;
#14766 = LINE ( 'NONE', #10714, #9888 ) ;
#14767 = DIRECTION ( 'NONE',  ( 1.000000000000000000, 0.000000000000000000, 0.000000000000000000 ) ) ;
#14768 = LINE ( 'NONE', #8225, #2780 ) ;
#14769 = DIRECTION ( 'NONE',  ( 0.000000000000000000, 0.000000000000000000, 1.000000000000000000 ) ) ;
#14770 = FACE_OUTER_BOUND ( 'NONE', #1842, .T. ) ;
#14771 = DIRECTION ( 'NONE',  ( 0.000000000000000000, 0.000000000000000000, 1.000000000000000000 ) ) ;
#14772 = ORIENTED_EDGE ( 'NONE', *, *, #16690, .T. ) ;
#14773 = EDGE_CURVE ( 'NONE', #14799, #8258, #12694, .T. ) ;
#14774 = EDGE_CURVE ( 'NONE', #1567, #13944, #11658, .T. ) ;
#14775 = EDGE_CURVE ( 'NONE', #16153, #3811, #8303, .T. ) ;
#14776 = FACE_OUTER_BOUND ( 'NONE', #3241, .T. ) ;
#14777 = EDGE_CURVE ( 'NONE', #9952, #2442, #12946, .T. ) ;
#14778 = DIRECTION ( 'NONE',  ( 1.000000000000000000, 0.000000000000000000, 0.000000000000000000 ) ) ;
#14779 = AXIS2_PLACEMENT_3D ( 'NONE', #2342, #16604, #16435 ) ;
#14780 = CARTESIAN_POINT ( 'NONE',  ( 1.286622718088548112E-12, 258.8496290447203023, 286.9685381829918924 ) ) ;
#14781 = ORIENTED_EDGE ( 'NONE', *, *, #7902, .T. ) ;
#14782 = CYLINDRICAL_SURFACE ( 'NONE', #893, 0.9999999999999965583 ) ;
#14783 = UNCERTAINTY_MEASURE_WITH_UNIT (LENGTH_MEASURE( 1.000000000000000082E-05 ), #16154, 'distance_accuracy_value', 'NONE');
#14784 = DIRECTION ( 'NONE',  ( -0.000000000000000000, -1.000000000000000000, -0.000000000000000000 ) ) ;
#14785 = CARTESIAN_POINT ( 'NONE',  ( -26.00000000000002842, 0.000000000000000000, -39.99999999999999289 ) ) ;
#14786 = ORIENTED_EDGE ( 'NONE', *, *, #14884, .F. ) ;
#14787 = CARTESIAN_POINT ( 'NONE',  ( -3.270000000000002238, 239.4632308570078294, 71.73739990498292229 ) ) ;
#14788 = CARTESIAN_POINT ( 'NONE',  ( -31.00000000000001776, 0.000000000000000000, 31.00000000000000000 ) ) ;
#14789 = DIRECTION ( 'NONE',  ( 0.000000000000000000, 0.000000000000000000, -1.000000000000000000 ) ) ;
#14790 = ORIENTED_EDGE ( 'NONE', *, *, #3116, .T. ) ;
#14791 = CIRCLE ( 'NONE', #2985, 14.27500000000000036 ) ;
#14792 = CARTESIAN_POINT ( 'NONE',  ( -55.99999999999989342, 473.6663340069157471, -526.8058340126048051 ) ) ;
#14793 = ORIENTED_EDGE ( 'NONE', *, *, #504, .F. ) ;
#14794 = EDGE_LOOP ( 'NONE', ( #10536, #11664, #8360, #6442 ) ) ;
#14795 = CARTESIAN_POINT ( 'NONE',  ( -46.99999999999988631, 473.6663340069157471, -517.8058340126048051 ) ) ;
#14796 = EDGE_CURVE ( 'NONE', #8672, #11572, #3100, .T. ) ;
#14797 = ORIENTED_EDGE ( 'NONE', *, *, #6702, .T. ) ;
#14798 = SHAPE_DEFINITION_REPRESENTATION ( #12232, #15920 ) ;
#14799 = VERTEX_POINT ( 'NONE', #16717 ) ;
#14800 = ORIENTED_EDGE ( 'NONE', *, *, #14240, .F. ) ;
#14801 = FACE_OUTER_BOUND ( 'NONE', #10583, .T. ) ;
#14802 = CARTESIAN_POINT ( 'NONE',  ( 2.265596578422603396E-15, -3.000000000000000000, 18.50000000000000000 ) ) ;
#14803 = EDGE_LOOP ( 'NONE', ( #1624, #2211 ) ) ;
#14804 = DIRECTION ( 'NONE',  ( 1.000000000000000000, -0.000000000000000000, -0.000000000000000000 ) ) ;
#14805 = EDGE_CURVE ( 'NONE', #15905, #5039, #5125, .T. ) ;
#14806 = CARTESIAN_POINT ( 'NONE',  ( 46.99999999999988631, 523.2161522479888163, -502.8936384967199729 ) ) ;
#14807 = ORIENTED_EDGE ( 'NONE', *, *, #11303, .F. ) ;
#14808 = VECTOR ( 'NONE', #2737, 1000.000000000000000 ) ;
#14809 = DIRECTION ( 'NONE',  ( 0.000000000000000000, 0.000000000000000000, 1.000000000000000000 ) ) ;
#14810 = EDGE_LOOP ( 'NONE', ( #7137, #14384, #16645, #13791 ) ) ;
#14811 = CARTESIAN_POINT ( 'NONE',  ( -9.000000000000001776, 2.755455298081549511E-15, -22.50000000000003908 ) ) ;
#14812 = CARTESIAN_POINT ( 'NONE',  ( -46.99999999999988631, 523.2161522479888163, -502.8936384967199729 ) ) ;
#14813 = VERTEX_POINT ( 'NONE', #14411 ) ;
#14814 = ORIENTED_EDGE ( 'NONE', *, *, #3876, .T. ) ;
#14815 = LINE ( 'NONE', #12152, #5913 ) ;
#14816 = ORIENTED_EDGE ( 'NONE', *, *, #8300, .F. ) ;
#14817 = AXIS2_PLACEMENT_3D ( 'NONE', #9849, #3484, #8727 ) ;
#14818 = EDGE_LOOP ( 'NONE', ( #16626, #6652, #13765, #8867, #14092 ) ) ;
#14819 = CARTESIAN_POINT ( 'NONE',  ( -37.00000000000000000, 68.00000000000000000, -22.99999999999999645 ) ) ;
#14820 = CARTESIAN_POINT ( 'NONE',  ( 449.9999999999998295, 135.5000000000000000, 3.000000000000000000 ) ) ;
#14821 = LINE ( 'NONE', #4263, #3132 ) ;
#14822 = LINE ( 'NONE', #6814, #2975 ) ;
#14823 = PRODUCT_DEFINITION_SHAPE ( 'NONE', 'NONE',  #16964 ) ;
#14824 = DIRECTION ( 'NONE',  ( 0.000000000000000000, 0.000000000000000000, 1.000000000000000000 ) ) ;
#14825 = DIRECTION ( 'NONE',  ( 0.000000000000000000, 0.000000000000000000, -1.000000000000000000 ) ) ;
#14826 = CARTESIAN_POINT ( 'NONE',  ( -34.99999999999996447, 11.00000000000000000, 40.00000000000000711 ) ) ;
#14827 = FACE_OUTER_BOUND ( 'NONE', #1220, .T. ) ;
#14828 = LINE ( 'NONE', #2712, #9124 ) ;
#14829 = VECTOR ( 'NONE', #3931, 1000.000000000000000 ) ;
#14830 = AXIS2_PLACEMENT_3D ( 'NONE', #1617, #11833, #5559 ) ;
#14831 = CARTESIAN_POINT ( 'NONE',  ( 19.99999999999995381, 3.000000000000000000, -36.99999999999999289 ) ) ;
#14832 = FILL_AREA_STYLE ('',( #14914 ) ) ;
#14834 = VERTEX_POINT ( 'NONE', #5290 ) ;
#14833 = VERTEX_POINT ( 'NONE', #2637 ) ;
#14835 = CARTESIAN_POINT ( 'NONE',  ( 0.3928280596732524055, 38.01925660030116205, 9.493865254640489582 ) ) ;
#14836 = CARTESIAN_POINT ( 'NONE',  ( 75.00000000000000000, 355.3192028797624857, -44.71049682360899169 ) ) ;
#14837 = EDGE_CURVE ( 'NONE', #6189, #13527, #4951, .T. ) ;
#14838 = PLANE ( 'NONE',  #12913 ) ;
#14839 = DIRECTION ( 'NONE',  ( 0.000000000000000000, 7.137148015447440312E-15, -1.000000000000000000 ) ) ;
#14840 = AXIS2_PLACEMENT_3D ( 'NONE', #1788, #13644, #16124 ) ;
#14841 = ORIENTED_EDGE ( 'NONE', *, *, #14674, .F. ) ;
#14842 = DIRECTION ( 'NONE',  ( 0.000000000000000000, 0.000000000000000000, -1.000000000000000000 ) ) ;
#14843 = ADVANCED_FACE ( 'NONE', ( #11566 ), #16800, .T. ) ;
#14844 = DIRECTION ( 'NONE',  ( -0.000000000000000000, 1.000000000000000000, -1.224646799147353207E-16 ) ) ;
#14845 = ORIENTED_EDGE ( 'NONE', *, *, #5587, .T. ) ;
#14846 = CARTESIAN_POINT ( 'NONE',  ( 40.00000000000000711, 19.00000000000000000, 25.99999999999999645 ) ) ;
#14847 = CARTESIAN_POINT ( 'NONE',  ( 40.00000000000003553, 3.000000000000000000, -25.99999999999999645 ) ) ;
#14848 = CARTESIAN_POINT ( 'NONE',  ( 31.81980515339464333, 8.000000000000000000, 31.81980515339463622 ) ) ;
#14849 = DIRECTION ( 'NONE',  ( 1.000000000000000000, 0.000000000000000000, 0.000000000000000000 ) ) ;
#14850 = SURFACE_STYLE_FILL_AREA ( #9614 ) ;
#14851 = DIRECTION ( 'NONE',  ( 0.000000000000000000, 0.000000000000000000, 1.000000000000000000 ) ) ;
#14852 = ORIENTED_EDGE ( 'NONE', *, *, #7641, .T. ) ;
#14853 = VECTOR ( 'NONE', #9062, 1000.000000000000227 ) ;
#14854 = DIRECTION ( 'NONE',  ( 1.000000000000000000, 0.000000000000000000, 0.000000000000000000 ) ) ;
#14855 = DIRECTION ( 'NONE',  ( -0.000000000000000000, -1.000000000000000000, 0.000000000000000000 ) ) ;
#14856 = ADVANCED_FACE ( 'NONE', ( #7689 ), #10377, .T. ) ;
#14857 = CARTESIAN_POINT ( 'NONE',  ( 39.99999999999999289, 10.00000000000000000, 18.99999999999999645 ) ) ;
#14858 = EDGE_LOOP ( 'NONE', ( #11576, #15820, #15303, #2023 ) ) ;
#14859 = LINE ( 'NONE', #6589, #11310 ) ;
#14860 = ADVANCED_FACE ( 'NONE', ( #13209 ), #13472, .T. ) ;
#14861 = EDGE_CURVE ( 'NONE', #777, #15604, #11326, .T. ) ;
#14862 = DIRECTION ( 'NONE',  ( -1.000000000000000000, -0.000000000000000000, -0.000000000000000000 ) ) ;
#14863 = ORIENTED_EDGE ( 'NONE', *, *, #409, .T. ) ;
#14864 = CARTESIAN_POINT ( 'NONE',  ( 45.00000000000000000, 523.2161522479893847, -590.5524132976893270 ) ) ;
#14865 = EDGE_CURVE ( 'NONE', #1506, #856, #2277, .T. ) ;
#14866 = LINE ( 'NONE', #8594, #10390 ) ;
#14867 = LINE ( 'NONE', #12291, #4829 ) ;
#14868 = ORIENTED_EDGE ( 'NONE', *, *, #13841, .T. ) ;
#14869 = AXIS2_PLACEMENT_3D ( 'NONE', #5017, #911, #12920 ) ;
#14870 = EDGE_LOOP ( 'NONE', ( #238, #5193, #6789, #329 ) ) ;
#14871 = ORIENTED_EDGE ( 'NONE', *, *, #6011, .T. ) ;
#14872 = DIRECTION ( 'NONE',  ( 0.000000000000000000, -1.000000000000000000, 0.000000000000000000 ) ) ;
#14873 = ORIENTED_EDGE ( 'NONE', *, *, #1726, .F. ) ;
#14874 = CARTESIAN_POINT ( 'NONE',  ( 0.000000000000000000, 380.0000000000000000, -1.364714047027919097 ) ) ;
#14875 = VECTOR ( 'NONE', #1041, 1000.000000000000000 ) ;
#14876 = ORIENTED_EDGE ( 'NONE', *, *, #8662, .F. ) ;
#14877 = ORIENTED_EDGE ( 'NONE', *, *, #14837, .F. ) ;
#14878 = DIRECTION ( 'NONE',  ( 1.000000000000000000, 0.000000000000000000, -0.000000000000000000 ) ) ;
#14879 = ADVANCED_FACE ( 'NONE', ( #8044 ), #5382, .F. ) ;
#14880 = CARTESIAN_POINT ( 'NONE',  ( 0.000000000000000000, 435.2933666400819561, -575.6295912558023247 ) ) ;
#14881 = ADVANCED_FACE ( 'NONE', ( #14759 ), #2982, .T. ) ;
#14882 = ORIENTED_EDGE ( 'NONE', *, *, #12634, .F. ) ;
#14883 = DIRECTION ( 'NONE',  ( 0.000000000000000000, 0.000000000000000000, -1.000000000000000000 ) ) ;
#14884 = EDGE_CURVE ( 'NONE', #5839, #11618, #14077, .T. ) ;
#14885 = DIRECTION ( 'NONE',  ( 0.000000000000000000, 0.000000000000000000, -1.000000000000000000 ) ) ;
#14886 = ORIENTED_EDGE ( 'NONE', *, *, #13715, .F. ) ;
#14887 = VECTOR ( 'NONE', #1272, 1000.000000000000000 ) ;
#14888 = CARTESIAN_POINT ( 'NONE',  ( 394.0000000000001137, 234.3157724647196289, -104.2090657433598011 ) ) ;
#14889 = ORIENTED_EDGE ( 'NONE', *, *, #535, .T. ) ;
#14890 = FILL_AREA_STYLE ('',( #6000 ) ) ;
#14891 = DIRECTION ( 'NONE',  ( 0.000000000000000000, 0.000000000000000000, 1.000000000000000000 ) ) ;
#14892 = ORIENTED_EDGE ( 'NONE', *, *, #3017, .F. ) ;
#14893 = VECTOR ( 'NONE', #10959, 1000.000000000000000 ) ;
#14894 = AXIS2_PLACEMENT_3D ( 'NONE', #14162, #5037, #10456 ) ;
#14895 = ORIENTED_EDGE ( 'NONE', *, *, #9413, .F. ) ;
#14896 = CARTESIAN_POINT ( 'NONE',  ( 37.18009836720080585, 275.4439001176564830, -17.00000000000000000 ) ) ;
#14897 = ORIENTED_EDGE ( 'NONE', *, *, #16141, .T. ) ;
#14898 = VECTOR ( 'NONE', #10339, 1000.000000000000000 ) ;
#14899 = ORIENTED_EDGE ( 'NONE', *, *, #9099, .F. ) ;
#14900 = DIRECTION ( 'NONE',  ( 0.000000000000000000, 0.000000000000000000, -1.000000000000000000 ) ) ;
#14901 = PLANE ( 'NONE',  #16489 ) ;
#14902 = LINE ( 'NONE', #12574, #4749 ) ;
#14903 = AXIS2_PLACEMENT_3D ( 'NONE', #5609, #15831, #5512 ) ;
#14904 = CARTESIAN_POINT ( 'NONE',  ( 175.0000000000000568, 515.4878487013597805, -571.7230258972048205 ) ) ;
#14905 = CIRCLE ( 'NONE', #3928, 36.50000000000000000 ) ;
#14906 = VECTOR ( 'NONE', #13799, 1000.000000000000000 ) ;
#14907 = DIRECTION ( 'NONE',  ( 0.000000000000000000, 1.000000000000000000, 0.000000000000000000 ) ) ;
#14908 = CARTESIAN_POINT ( 'NONE',  ( -3.269999999998768114, 193.4898140233619017, 37.52989836422146652 ) ) ;
#14909 = DIRECTION ( 'NONE',  ( -1.000000000000000000, -0.000000000000000000, -0.000000000000000000 ) ) ;
#14910 = CARTESIAN_POINT ( 'NONE',  ( -55.99999999999989342, 473.6663340069157471, -531.5012393965008641 ) ) ;
#14911 = DIRECTION ( 'NONE',  ( -1.000000000000000000, 0.000000000000000000, -0.000000000000000000 ) ) ;
#14912 = CONICAL_SURFACE ( 'NONE', #8032, 12.97499999999999964, 0.5543074962015517304 ) ;
#14913 = CARTESIAN_POINT ( 'NONE',  ( 0.000000000000000000, 3.000000000000000000, -36.50000000000000000 ) ) ;
#14914 = FILL_AREA_STYLE_COLOUR ( '', #10971 ) ;
#14916 = ORIENTED_EDGE ( 'NONE', *, *, #13418, .T. ) ;
#14915 = VERTEX_POINT ( 'NONE', #15858 ) ;
#14917 = CIRCLE ( 'NONE', #11616, 10.00000000000000178 ) ;
#14918 = LINE ( 'NONE', #5723, #3716 ) ;
#14919 = AXIS2_PLACEMENT_3D ( 'NONE', #7485, #5001, #8886 ) ;
#14920 = AXIS2_PLACEMENT_3D ( 'NONE', #1922, #7145, #8537 ) ;
#14921 = EDGE_CURVE ( 'NONE', #9305, #6283, #14925, .T. ) ;
#14922 = DIRECTION ( 'NONE',  ( 1.000000000000000000, -0.000000000000000000, -0.000000000000000000 ) ) ;
#14923 = CIRCLE ( 'NONE', #2024, 4.695405383896011919 ) ;
#14924 = CARTESIAN_POINT ( 'NONE',  ( 5.044974746830580337, 0.000000000000000000, 0.000000000000000000 ) ) ;
#14925 = LINE ( 'NONE', #4101, #367 ) ;
#14926 = CIRCLE ( 'NONE', #116, 13.69540538389601991 ) ;
#14927 = ORIENTED_EDGE ( 'NONE', *, *, #13983, .F. ) ;
#14928 = ADVANCED_FACE ( 'NONE', ( #9340 ), #6920, .T. ) ;
#14929 = AXIS2_PLACEMENT_3D ( 'NONE', #5999, #11245, #9883 ) ;
#14930 = AXIS2_PLACEMENT_3D ( 'NONE', #16265, #2959, #8013 ) ;
#14931 = LINE ( 'NONE', #3170, #16641 ) ;
#14932 = ORIENTED_EDGE ( 'NONE', *, *, #11410, .T. ) ;
#14933 = CARTESIAN_POINT ( 'NONE',  ( -0.3928280596732490748, 62.98074339969887347, 9.493865254640493134 ) ) ;
#14934 = AXIS2_PLACEMENT_3D ( 'NONE', #9128, #7910, #206 ) ;
#14935 = CARTESIAN_POINT ( 'NONE',  ( 0.7366000000000039183, 192.7170024689980323, 37.20452120302198296 ) ) ;
#14936 = CYLINDRICAL_SURFACE ( 'NONE', #9923, 3.299999999999997158 ) ;
#14937 = PRODUCT_DEFINITION ( 'UNKNOWN', '', #15223, #13946 ) ;
#14938 = VECTOR ( 'NONE', #14872, 1000.000000000000000 ) ;
#14939 = DIRECTION ( 'NONE',  ( 1.000000000000000000, 0.000000000000000000, 0.000000000000000000 ) ) ;
#14940 = DIRECTION ( 'NONE',  ( 0.000000000000000000, 0.000000000000000000, -1.000000000000000000 ) ) ;
#14941 = VERTEX_POINT ( 'NONE', #14579 ) ;
#14942 = FACE_OUTER_BOUND ( 'NONE', #9239, .T. ) ;
#14943 = EDGE_CURVE ( 'NONE', #15471, #5942, #6829, .T. ) ;
#14944 =( GEOMETRIC_REPRESENTATION_CONTEXT ( 3 ) GLOBAL_UNCERTAINTY_ASSIGNED_CONTEXT ( ( #15175 ) ) GLOBAL_UNIT_ASSIGNED_CONTEXT ( ( #1387, #9123, #113 ) ) REPRESENTATION_CONTEXT ( 'NONE', 'WORKASPACE' ) );
#14945 = DIRECTION ( 'NONE',  ( -0.000000000000000000, 1.000000000000000000, -0.000000000000000000 ) ) ;
#14946 = VECTOR ( 'NONE', #14055, 1000.000000000000000 ) ;
#14947 = ORIENTED_EDGE ( 'NONE', *, *, #3935, .T. ) ;
#14948 = AXIS2_PLACEMENT_3D ( 'NONE', #2652, #15373, #3609 ) ;
#14949 = FACE_BOUND ( 'NONE', #10276, .T. ) ;
#14950 = CARTESIAN_POINT ( 'NONE',  ( -31.00000000000006395, 19.00000000000000000, 20.99999999999998934 ) ) ;
#14951 = ORIENTED_EDGE ( 'NONE', *, *, #13931, .T. ) ;
#14952 = CARTESIAN_POINT ( 'NONE',  ( -55.99999999999989342, 523.2161522479888163, -502.8936384967199729 ) ) ;
#14953 = CARTESIAN_POINT ( 'NONE',  ( 4.286263797015737285E-15, -3.000000000000000000, -35.00000000000000711 ) ) ;
#14954 = DIRECTION ( 'NONE',  ( 0.000000000000000000, 0.000000000000000000, 1.000000000000000000 ) ) ;
#14955 = ORIENTED_EDGE ( 'NONE', *, *, #10392, .T. ) ;
#14956 = EDGE_LOOP ( 'NONE', ( #10079, #1828, #1493, #10515 ) ) ;
#14957 = ADVANCED_FACE ( 'NONE', ( #9598 ), #419, .F. ) ;
#14958 = DIRECTION ( 'NONE',  ( 0.000000000000000000, 1.000000000000000000, 0.000000000000000000 ) ) ;
#14959 = ORIENTED_EDGE ( 'NONE', *, *, #9707, .T. ) ;
#14960 = ORIENTED_EDGE ( 'NONE', *, *, #4384, .T. ) ;
#14961 = CARTESIAN_POINT ( 'NONE',  ( 46.99999999999988631, 523.2161522479893847, -590.5524132976893270 ) ) ;
#14962 = CIRCLE ( 'NONE', #3434, 187.4999999999998863 ) ;
#14963 = PRODUCT_CONTEXT ( 'NONE', #5331, 'mechanical' ) ;
#14964 = ADVANCED_FACE ( 'NONE', ( #328 ), #12006, .T. ) ;
#14965 = ADVANCED_FACE ( 'NONE', ( #6666 ), #9429, .F. ) ;
#14966 = PRODUCT ( 'Servo-Bas', 'Servo-Bas', '', ( #2069 ) ) ;
#14967 = VERTEX_POINT ( 'NONE', #10708 ) ;
#14968 = CARTESIAN_POINT ( 'NONE',  ( -55.99999999999989342, 549.5810598491746077, -522.8108303813202156 ) ) ;
#14969 = ORIENTED_EDGE ( 'NONE', *, *, #3843, .F. ) ;
#14970 = CARTESIAN_POINT ( 'NONE',  ( 22.99999999999998224, 10.00000000000000000, -31.00000000000003197 ) ) ;
#14971 = FACE_OUTER_BOUND ( 'NONE', #14420, .T. ) ;
#14972 = VERTEX_POINT ( 'NONE', #2902 ) ;
#14973 = VECTOR ( 'NONE', #10294, 1000.000000000000114 ) ;
#14974 = FACE_BOUND ( 'NONE', #9033, .T. ) ;
#14975 = DIRECTION ( 'NONE',  ( 0.000000000000000000, 0.000000000000000000, 1.000000000000000000 ) ) ;
#14976 = ORIENTED_EDGE ( 'NONE', *, *, #2151, .T. ) ;
#14977 = ADVANCED_FACE ( 'NONE', ( #13559 ), #8138, .T. ) ;
#14978 = VERTEX_POINT ( 'NONE', #12088 ) ;
#14979 = LINE ( 'NONE', #11021, #4483 ) ;
#14980 = ORIENTED_EDGE ( 'NONE', *, *, #9934, .F. ) ;
#14981 = ORIENTED_EDGE ( 'NONE', *, *, #5174, .F. ) ;
#14982 = EDGE_CURVE ( 'NONE', #5425, #7243, #12268, .T. ) ;
#14983 = EDGE_CURVE ( 'NONE', #13664, #963, #9965, .T. ) ;
#14984 = CIRCLE ( 'NONE', #176, 3.300000000000011369 ) ;
#14985 = EDGE_CURVE ( 'NONE', #13726, #856, #13719, .T. ) ;
#14986 = EDGE_CURVE ( 'NONE', #175, #9495, #16378, .T. ) ;
#14987 = ORIENTED_EDGE ( 'NONE', *, *, #6342, .T. ) ;
#14988 = VERTEX_POINT ( 'NONE', #6052 ) ;
#14989 = CARTESIAN_POINT ( 'NONE',  ( 34.00000000000002842, 3.000000000000000000, 23.00000000000000355 ) ) ;
#14990 = DIRECTION ( 'NONE',  ( -0.01502673813723916403, 0.9998870921963913805, 0.000000000000000000 ) ) ;
#14991 = CARTESIAN_POINT ( 'NONE',  ( 54.99999999999999289, 515.4878487013597805, -461.7230258972048205 ) ) ;
#14992 = CARTESIAN_POINT ( 'NONE',  ( 44.68009836720079875, 352.3758082234937206, -17.00000000000000000 ) ) ;
#14993 = CARTESIAN_POINT ( 'NONE',  ( 25.99999999999997868, 10.00000000000000000, 40.00000000000000711 ) ) ;
#14994 = VECTOR ( 'NONE', #11397, 1000.000000000000000 ) ;
#14995 = FACE_OUTER_BOUND ( 'NONE', #7013, .T. ) ;
#14996 = CIRCLE ( 'NONE', #1268, 4.695405383896011919 ) ;
#14997 = CARTESIAN_POINT ( 'NONE',  ( -45.00000000000000000, 515.4878487013597805, -546.7230258972048205 ) ) ;
#14998 = VERTEX_POINT ( 'NONE', #15011 ) ;
#14999 = CARTESIAN_POINT ( 'NONE',  ( 10.00000000000000000, 435.2933666400819561, -550.3792044179907634 ) ) ;
#15000 = DIRECTION ( 'NONE',  ( 0.000000000000000000, 0.000000000000000000, 1.000000000000000000 ) ) ;
#15001 = B_SPLINE_CURVE_WITH_KNOTS ( 'NONE', 3,
 ( #11146, #13975, #7017, #2116, #1949, #16383, #3251, #15015, #15090, #9946, #8658, #840, #3500, #14933, #7172, #11226 ),
 .UNSPECIFIED., .F., .F.,
 ( 4, 2, 2, 2, 2, 2, 2, 4 ),
 ( 0.000000000000000000, 0.0005901654530283981324, 0.001180330906056796265, 0.001770496359085194180, 0.002360661812113592530, 0.003540992718170401805, 0.004131158171198806225, 0.004721323624227211080 ),
 .UNSPECIFIED. ) ;
#15002 = DIRECTION ( 'NONE',  ( -6.123031769111888756E-17, 1.000000000000000000, 3.749151804555344967E-33 ) ) ;
#15003 = FACE_OUTER_BOUND ( 'NONE', #7562, .T. ) ;
#15005 = EDGE_LOOP ( 'NONE', ( #4096, #374, #559, #5344 ) ) ;
#15004 = ORIENTED_EDGE ( 'NONE', *, *, #15086, .T. ) ;
#15006 = DIRECTION ( 'NONE',  ( -0.000000000000000000, -1.000000000000000000, -0.000000000000000000 ) ) ;
#15007 = EDGE_CURVE ( 'NONE', #6541, #11430, #2546, .T. ) ;
#15008 = VECTOR ( 'NONE', #5634, 1000.000000000000000 ) ;
#15009 = CIRCLE ( 'NONE', #7576, 187.4999999999998863 ) ;
#15010 = DIRECTION ( 'NONE',  ( 0.000000000000000000, 0.000000000000000000, -1.000000000000000000 ) ) ;
#15011 = CARTESIAN_POINT ( 'NONE',  ( -46.99999999999988631, 473.6663340069158039, -575.6402177818052905 ) ) ;
#15012 = ORIENTED_EDGE ( 'NONE', *, *, #15592, .T. ) ;
#15013 = PLANE ( 'NONE',  #14182 ) ;
#15014 = EDGE_LOOP ( 'NONE', ( #13242, #15528 ) ) ;
#15015 = CARTESIAN_POINT ( 'NONE',  ( -2.383743612111324239, 61.83195493428745237, 9.196765735797573171 ) ) ;
#15016 = CARTESIAN_POINT ( 'NONE',  ( -2.792885358475956092, 191.4523525084761673, 37.59942507683140178 ) ) ;
#15017 = DIRECTION ( 'NONE',  ( 0.000000000000000000, 0.000000000000000000, -1.000000000000000000 ) ) ;
#15018 = DIRECTION ( 'NONE',  ( 1.000000000000000000, 0.000000000000000000, -0.000000000000000000 ) ) ;
#15019 = DIRECTION ( 'NONE',  ( 0.000000000000000000, 0.000000000000000000, -1.000000000000000000 ) ) ;
#15020 = ORIENTED_EDGE ( 'NONE', *, *, #5280, .F. ) ;
#15021 = DIRECTION ( 'NONE',  ( 1.000000000000000000, 0.000000000000000000, 0.000000000000000000 ) ) ;
#15022 = CARTESIAN_POINT ( 'NONE',  ( 45.00000000000000000, 523.2161522479888163, -502.8936384967199729 ) ) ;
#15023 = SURFACE_STYLE_FILL_AREA ( #5989 ) ;
#15024 = MECHANICAL_DESIGN_GEOMETRIC_PRESENTATION_REPRESENTATION (  '', ( #222 ), #7601 ) ;
#15025 = ORIENTED_EDGE ( 'NONE', *, *, #7489, .T. ) ;
#15026 = DIRECTION ( 'NONE',  ( -1.000000000000000000, -0.000000000000000000, 3.854941057726258312E-16 ) ) ;
#15027 = ADVANCED_FACE ( 'NONE', ( #1944 ), #16624, .T. ) ;
#15028 = DIRECTION ( 'NONE',  ( 0.000000000000000000, 1.000000000000000000, 0.000000000000000000 ) ) ;
#15029 = ORIENTED_EDGE ( 'NONE', *, *, #11938, .F. ) ;
#15030 = DIRECTION ( 'NONE',  ( -1.000000000000000000, 0.000000000000000000, 0.000000000000000000 ) ) ;
#15031 = LINE ( 'NONE', #13744, #518 ) ;
#15032 = DIRECTION ( 'NONE',  ( -1.000000000000000000, -0.000000000000000000, -0.000000000000000000 ) ) ;
#15033 = ORIENTED_EDGE ( 'NONE', *, *, #15156, .F. ) ;
#15034 = LINE ( 'NONE', #8597, #11090 ) ;
#15035 = ORIENTED_EDGE ( 'NONE', *, *, #10607, .T. ) ;
#15036 = VERTEX_POINT ( 'NONE', #12424 ) ;
#15037 = CARTESIAN_POINT ( 'NONE',  ( 10.00000000000000000, 309.2289037985890445, -143.5198051533984085 ) ) ;
#15038 = AXIS2_PLACEMENT_3D ( 'NONE', #8167, #4314, #10483 ) ;
#15039 = APPLICATION_PROTOCOL_DEFINITION ( 'draft international standard', 'automotive_design', 1998, #7403 ) ;
#15040 = CARTESIAN_POINT ( 'NONE',  ( 29.68009836720079875, 352.3758082234937206, 0.000000000000000000 ) ) ;
#15041 = ORIENTED_EDGE ( 'NONE', *, *, #15802, .T. ) ;
#15042 = ADVANCED_FACE ( 'NONE', ( #667 ), #8651, .F. ) ;
#15043 = CARTESIAN_POINT ( 'NONE',  ( 7.000000000000000000, 17.52499999999999858, 0.000000000000000000 ) ) ;
#15044 = DIRECTION ( 'NONE',  ( -1.000000000000000000, -0.000000000000000000, -0.000000000000000000 ) ) ;
#15045 = EDGE_LOOP ( 'NONE', ( #14157, #2776 ) ) ;
#15046 = CARTESIAN_POINT ( 'NONE',  ( 1.163414459189985485E-15, 66.00000000000000000, 9.500000000000000000 ) ) ;
#15047 = AXIS2_PLACEMENT_3D ( 'NONE', #15205, #7113, #13832 ) ;
#15048 = LINE ( 'NONE', #799, #13914 ) ;
#15049 = ORIENTED_EDGE ( 'NONE', *, *, #13102, .T. ) ;
#15050 = EDGE_CURVE ( 'NONE', #16578, #748, #8736, .T. ) ;
#15051 = DIRECTION ( 'NONE',  ( -2.943801717315837579E-15, 0.9950371902099846011, 0.09950371902104368504 ) ) ;
#15052 = ORIENTED_EDGE ( 'NONE', *, *, #689, .T. ) ;
#15053 = ORIENTED_EDGE ( 'NONE', *, *, #14392, .T. ) ;
#15054 = VERTEX_POINT ( 'NONE', #8480 ) ;
#15055 = CIRCLE ( 'NONE', #9031, 84.99999999999997158 ) ;
#15056 = EDGE_LOOP ( 'NONE', ( #922, #7141, #10772, #6244, #730, #11157 ) ) ;
#15057 = ORIENTED_EDGE ( 'NONE', *, *, #5308, .F. ) ;
#15058 = CARTESIAN_POINT ( 'NONE',  ( 394.0000000000001137, 240.7889724647196488, -104.9456657433598110 ) ) ;
#15059 = EDGE_CURVE ( 'NONE', #2588, #12483, #3493, .T. ) ;
#15060 = ADVANCED_FACE ( 'NONE', ( #10104 ), #10023, .F. ) ;
#15061 = CARTESIAN_POINT ( 'NONE',  ( -26.00000000000000000, 19.00000000000000000, -40.00000000000000711 ) ) ;
#15062 = DIRECTION ( 'NONE',  ( 0.000000000000000000, 0.000000000000000000, -1.000000000000000000 ) ) ;
#15063 = CIRCLE ( 'NONE', #5771, 4.695405383896011919 ) ;
#15064 = LINE ( 'NONE', #5711, #236 ) ;
#15065 = LINE ( 'NONE', #13703, #7481 ) ;
#15066 = ADVANCED_FACE ( 'NONE', ( #5806, #3247 ), #7088, .T. ) ;
#15067 = EDGE_CURVE ( 'NONE', #13527, #11643, #3114, .T. ) ;
#15068 = EDGE_CURVE ( 'NONE', #13306, #3723, #13645, .T. ) ;
#15069 = CARTESIAN_POINT ( 'NONE',  ( 75.00000000000000000, 355.3192028797624857, -44.71049682360899169 ) ) ;
#15070 = EDGE_CURVE ( 'NONE', #5898, #9012, #5018, .T. ) ;
#15071 = CARTESIAN_POINT ( 'NONE',  ( 46.99999999999988631, 493.2350855268092573, -585.2659423243250103 ) ) ;
#15072 = ORIENTED_EDGE ( 'NONE', *, *, #4637, .F. ) ;
#15073 = CARTESIAN_POINT ( 'NONE',  ( -45.00000000000000000, 473.6663340069158039, -548.2494070140132862 ) ) ;
#15074 = DIRECTION ( 'NONE',  ( -1.000000000000000000, -0.000000000000000000, -0.000000000000000000 ) ) ;
#15075 = DIRECTION ( 'NONE',  ( 0.000000000000000000, 0.000000000000000000, 1.000000000000000000 ) ) ;
#15076 = FACE_OUTER_BOUND ( 'NONE', #10312, .T. ) ;
#15078 = ORIENTED_EDGE ( 'NONE', *, *, #13720, .F. ) ;
#15077 = VERTEX_POINT ( 'NONE', #12510 ) ;
#15079 = DIRECTION ( 'NONE',  ( 1.000000000000000000, 0.000000000000000000, 0.000000000000000000 ) ) ;
#15080 = CIRCLE ( 'NONE', #15889, 15.00000000000000000 ) ;
#15081 = VERTEX_POINT ( 'NONE', #16295 ) ;
#15082 = CARTESIAN_POINT ( 'NONE',  ( 21.99999999999998224, 6.000000000000000000, -31.99999999999998579 ) ) ;
#15083 = CARTESIAN_POINT ( 'NONE',  ( 31.00000000000000000, 11.00000000000000000, -31.00000000000000355 ) ) ;
#15084 = VERTEX_POINT ( 'NONE', #4533 ) ;
#15085 = CARTESIAN_POINT ( 'NONE',  ( 45.00000000000000000, 473.6663340069158039, -561.9448123979092315 ) ) ;
#15086 = EDGE_CURVE ( 'NONE', #155, #12375, #14345, .T. ) ;
#15087 = VECTOR ( 'NONE', #16368, 1000.000000000000000 ) ;
#15088 = CYLINDRICAL_SURFACE ( 'NONE', #12266, 18.50000000000000000 ) ;
#15089 = ORIENTED_EDGE ( 'NONE', *, *, #504, .T. ) ;
#15090 = CARTESIAN_POINT ( 'NONE',  ( -2.257948793614859451, 61.98480561674775657, 9.228844315538689003 ) ) ;
#15091 = VECTOR ( 'NONE', #9346, 1000.000000000000000 ) ;
#15092 = EDGE_CURVE ( 'NONE', #851, #16527, #4679, .T. ) ;
#15093 = DIRECTION ( 'NONE',  ( 0.000000000000000000, 0.000000000000000000, -1.000000000000000000 ) ) ;
#15094 = LINE ( 'NONE', #8574, #7708 ) ;
#15095 = DIRECTION ( 'NONE',  ( 0.000000000000000000, 0.000000000000000000, -1.000000000000000000 ) ) ;
#15096 = CARTESIAN_POINT ( 'NONE',  ( 0.3499999999999999778, -18.17500000000000071, 2.225795557450314789E-15 ) ) ;
#15097 = EDGE_LOOP ( 'NONE', ( #1587, #5679, #7032, #14877 ) ) ;
#15098 = DIRECTION ( 'NONE',  ( 0.000000000000000000, 0.000000000000000000, -1.000000000000000000 ) ) ;
#15099 = AXIS2_PLACEMENT_3D ( 'NONE', #13961, #2184, #6369 ) ;
#15100 = DIRECTION ( 'NONE',  ( 0.000000000000000000, 0.000000000000000000, -1.000000000000000000 ) ) ;
#15101 = VERTEX_POINT ( 'NONE', #3411 ) ;
#15102 = DIRECTION ( 'NONE',  ( 1.000000000000000000, 0.000000000000000000, 0.000000000000000000 ) ) ;
#15103 = ORIENTED_EDGE ( 'NONE', *, *, #5560, .T. ) ;
#15104 = DIRECTION ( 'NONE',  ( -1.000000000000000000, -0.000000000000000000, -0.000000000000000000 ) ) ;
#15105 = PLANE ( 'NONE',  #3743 ) ;
#15106 = EDGE_LOOP ( 'NONE', ( #9718, #5243, #12993, #14236 ) ) ;
#15107 = DIRECTION ( 'NONE',  ( -1.000000000000000000, -0.000000000000000000, -0.000000000000000000 ) ) ;
#15108 = LINE ( 'NONE', #5752, #13685 ) ;
#15109 = DIRECTION ( 'NONE',  ( -0.000000000000000000, 0.000000000000000000, 1.000000000000000000 ) ) ;
#15110 = ORIENTED_EDGE ( 'NONE', *, *, #12660, .T. ) ;
#15111 = VECTOR ( 'NONE', #9933, 1000.000000000000000 ) ;
#15112 = CARTESIAN_POINT ( 'NONE',  ( 35.99999999999999289, 6.000000000000000000, 21.99999999999999645 ) ) ;
#15113 = ORIENTED_EDGE ( 'NONE', *, *, #10974, .T. ) ;
#15114 = ORIENTED_EDGE ( 'NONE', *, *, #15704, .F. ) ;
#15115 = CARTESIAN_POINT ( 'NONE',  ( -20.00000000000003197, 3.000000000000000000, 37.00000000000000711 ) ) ;
#15116 = APPLICATION_PROTOCOL_DEFINITION ( 'draft international standard', 'automotive_design', 1998, #306 ) ;
#15117 = SHAPE_REPRESENTATION_RELATIONSHIP ( 'NONE' , 'NONE' ,  #135, #8557 ) ;
#15118 = DIRECTION ( 'NONE',  ( 1.000000000000000000, -0.000000000000000000, -0.000000000000000000 ) ) ;
#15119 = CIRCLE ( 'NONE', #16225, 18.50000000000000000 ) ;
#15120 = VERTEX_POINT ( 'NONE', #2110 ) ;
#15121 = CYLINDRICAL_SURFACE ( 'NONE', #12404, 2.500000000000002220 ) ;
#15122 = DIRECTION ( 'NONE',  ( -0.000000000000000000, -1.000000000000000000, -0.000000000000000000 ) ) ;
#15123 = ORIENTED_EDGE ( 'NONE', *, *, #6337, .T. ) ;
#15124 = AXIS2_PLACEMENT_3D ( 'NONE', #5212, #1704, #1539 ) ;
#15125 = LINE ( 'NONE', #11260, #16284 ) ;
#15126 = CIRCLE ( 'NONE', #3341, 18.49999999999998934 ) ;
#15127 = CIRCLE ( 'NONE', #1139, 13.69540538389596485 ) ;
#15128 = DIRECTION ( 'NONE',  ( -0.000000000000000000, -1.000000000000000000, -0.000000000000000000 ) ) ;
#15129 = VERTEX_POINT ( 'NONE', #7340 ) ;
#15130 = DIRECTION ( 'NONE',  ( 0.000000000000000000, 0.000000000000000000, 1.000000000000000000 ) ) ;
#15131 = ORIENTED_EDGE ( 'NONE', *, *, #11478, .T. ) ;
#15132 = VERTEX_POINT ( 'NONE', #834 ) ;
#15133 = VECTOR ( 'NONE', #4996, 1000.000000000000114 ) ;
#15134 = EDGE_CURVE ( 'NONE', #5278, #16003, #12766, .T. ) ;
#15135 = ORIENTED_EDGE ( 'NONE', *, *, #10123, .T. ) ;
#15136 = VECTOR ( 'NONE', #9443, 1000.000000000000000 ) ;
#15137 = CIRCLE ( 'NONE', #8566, 3.300000000000025135 ) ;
#15138 = VECTOR ( 'NONE', #15674, 1000.000000000000000 ) ;
#15139 = TOROIDAL_SURFACE ( 'NONE', #16787, 4.695405383895982609, 9.000000000000000000 ) ;
#15140 = ORIENTED_EDGE ( 'NONE', *, *, #10235, .T. ) ;
#15141 = ADVANCED_FACE ( 'NONE', ( #11546 ), #16784, .F. ) ;
#15142 = VERTEX_POINT ( 'NONE', #5107 ) ;
#15143 = CARTESIAN_POINT ( 'NONE',  ( -2.259918635623970218, 39.01734001413205277, 9.228371864727252571 ) ) ;
#15144 = CARTESIAN_POINT ( 'NONE',  ( -34.99999999999998579, 0.000000000000000000, 23.50000000000000711 ) ) ;
#15145 = DIRECTION ( 'NONE',  ( 1.000000000000000000, 0.000000000000000000, 0.000000000000000000 ) ) ;
#15146 = AXIS2_PLACEMENT_3D ( 'NONE', #2834, #13328, #1886 ) ;
#15147 = DIRECTION ( 'NONE',  ( -0.000000000000000000, 0.000000000000000000, -1.000000000000000000 ) ) ;
#15148 = DIRECTION ( 'NONE',  ( 1.000000000000000000, 6.123031769111888756E-17, 7.900838015626929923E-17 ) ) ;
#15149 = DIRECTION ( 'NONE',  ( 1.000000000000000000, -0.000000000000000000, -0.000000000000000000 ) ) ;
#15150 = DIRECTION ( 'NONE',  ( -1.000000000000000000, 0.000000000000000000, 0.000000000000000000 ) ) ;
#15151 = DIRECTION ( 'NONE',  ( 1.000000000000000000, 0.000000000000000000, -0.000000000000000000 ) ) ;
#15152 = AXIS2_PLACEMENT_3D ( 'NONE', #15533, #15776, #6399 ) ;
#15153 = ORIENTED_EDGE ( 'NONE', *, *, #10742, .T. ) ;
#15154 = DIRECTION ( 'NONE',  ( -1.000000000000000000, -0.000000000000000000, -0.000000000000000000 ) ) ;
#15155 = CARTESIAN_POINT ( 'NONE',  ( 40.00000000000000711, 0.000000000000000000, 34.99999999999997868 ) ) ;
#15156 = EDGE_CURVE ( 'NONE', #1644, #11171, #1077, .T. ) ;
#15157 = LINE ( 'NONE', #13078, #11623 ) ;
#15158 = EDGE_CURVE ( 'NONE', #3345, #14135, #8873, .T. ) ;
#15159 = PLANE ( 'NONE',  #8509 ) ;
#15161 = ORIENTED_EDGE ( 'NONE', *, *, #13751, .T. ) ;
#15160 = EDGE_LOOP ( 'NONE', ( #11415, #7317, #10132, #3808 ) ) ;
#15162 = CIRCLE ( 'NONE', #9687, 2.999999999999999112 ) ;
#15163 = LINE ( 'NONE', #12263, #1519 ) ;
#15164 = ORIENTED_EDGE ( 'NONE', *, *, #15067, .F. ) ;
#15165 = ADVANCED_FACE ( 'NONE', ( #11466 ), #14143, .F. ) ;
#15166 = EDGE_CURVE ( 'NONE', #5839, #9380, #3911, .T. ) ;
#15167 = EDGE_CURVE ( 'NONE', #3191, #11441, #3577, .T. ) ;
#15168 =( LENGTH_UNIT ( ) NAMED_UNIT ( * ) SI_UNIT ( .MILLI., .METRE. ) );
#15169 = EDGE_CURVE ( 'NONE', #15577, #478, #10281, .T. ) ;
#15170 = VECTOR ( 'NONE', #1066, 1000.000000000000000 ) ;
#15171 = AXIS2_PLACEMENT_3D ( 'NONE', #1529, #12180, #16204 ) ;
#15172 = DIRECTION ( 'NONE',  ( 0.000000000000000000, 1.000000000000000000, 0.000000000000000000 ) ) ;
#15173 = DIRECTION ( 'NONE',  ( 0.000000000000000000, 1.000000000000000000, 0.000000000000000000 ) ) ;
#15174 = EDGE_LOOP ( 'NONE', ( #4801, #9927, #7905, #1297 ) ) ;
#15175 = UNCERTAINTY_MEASURE_WITH_UNIT (LENGTH_MEASURE( 1.000000000000000082E-05 ), #1387, 'distance_accuracy_value', 'NONE');
#15176 = PLANE ( 'NONE',  #9465 ) ;
#15177 = VECTOR ( 'NONE', #122, 1000.000000000000000 ) ;
#15178 = DIRECTION ( 'NONE',  ( 1.000000000000000000, -0.000000000000000000, 1.631319816340925608E-17 ) ) ;
#15179 = ORIENTED_EDGE ( 'NONE', *, *, #1183, .F. ) ;
#15180 = PLANE ( 'NONE',  #9620 ) ;
#15181 = DIRECTION ( 'NONE',  ( 1.000000000000000000, -0.000000000000000000, -0.000000000000000000 ) ) ;
#15182 = DIRECTION ( 'NONE',  ( 0.000000000000000000, 1.000000000000000000, 0.000000000000000000 ) ) ;
#15183 = AXIS2_PLACEMENT_3D ( 'NONE', #8972, #3647, #2509 ) ;
#15184 = VECTOR ( 'NONE', #12657, 1000.000000000000000 ) ;
#15185 = EDGE_CURVE ( 'NONE', #16479, #6787, #2529, .T. ) ;
#15186 = DIRECTION ( 'NONE',  ( -0.000000000000000000, -0.000000000000000000, 1.000000000000000000 ) ) ;
#15187 = TOROIDAL_SURFACE ( 'NONE', #6119, 4.695405383895982609, 9.000000000000000000 ) ;
#15188 = DIRECTION ( 'NONE',  ( 0.000000000000000000, 0.000000000000000000, -1.000000000000000000 ) ) ;
#15189 = ORIENTED_EDGE ( 'NONE', *, *, #5724, .F. ) ;
#15190 = DIRECTION ( 'NONE',  ( 0.000000000000000000, 0.000000000000000000, -1.000000000000000000 ) ) ;
#15191 = EDGE_CURVE ( 'NONE', #4106, #12123, #10242, .T. ) ;
#15192 = CIRCLE ( 'NONE', #8045, 13.69540538389599682 ) ;
#15193 = ADVANCED_FACE ( 'NONE', ( #7507 ), #1334, .F. ) ;
#15194 = FACE_OUTER_BOUND ( 'NONE', #11089, .T. ) ;
#15195 = EDGE_CURVE ( 'NONE', #687, #3292, #14223, .T. ) ;
#15196 = ORIENTED_EDGE ( 'NONE', *, *, #9077, .T. ) ;
#15197 = CARTESIAN_POINT ( 'NONE',  ( -37.00000000000000711, 10.00000000000000000, 23.00000000000000000 ) ) ;
#15198 = ORIENTED_EDGE ( 'NONE', *, *, #1420, .F. ) ;
#15199 =( GEOMETRIC_REPRESENTATION_CONTEXT ( 3 ) GLOBAL_UNCERTAINTY_ASSIGNED_CONTEXT ( ( #7595 ) ) GLOBAL_UNIT_ASSIGNED_CONTEXT ( ( #11678, #3703, #15794 ) ) REPRESENTATION_CONTEXT ( 'NONE', 'WORKASPACE' ) );
#15200 = DIRECTION ( 'NONE',  ( -1.803905316987902527E-16, 1.000000000000000000, 0.000000000000000000 ) ) ;
#15201 = DIRECTION ( 'NONE',  ( -1.000000000000000000, 0.000000000000000000, 0.000000000000000000 ) ) ;
#15202 = EDGE_LOOP ( 'NONE', ( #1346, #7832, #7232, #6744 ) ) ;
#15203 = LINE ( 'NONE', #8677, #16572 ) ;
#15204 = VECTOR ( 'NONE', #11737, 1000.000000000000000 ) ;
#15205 = CARTESIAN_POINT ( 'NONE',  ( 39.41161623800082481, 323.9612906317821057, -6.736600000000000144 ) ) ;
#15206 = DIRECTION ( 'NONE',  ( 1.000000000000000000, 0.000000000000000000, -0.000000000000000000 ) ) ;
#15207 = EDGE_LOOP ( 'NONE', ( #9324, #14845, #11085, #13077 ) ) ;
#15208 = AXIS2_PLACEMENT_3D ( 'NONE', #15616, #15449, #6320 ) ;
#15209 = CARTESIAN_POINT ( 'NONE',  ( 44.68009836720079875, 352.3758082234937206, 0.000000000000000000 ) ) ;
#15210 = SURFACE_SIDE_STYLE ('',( #11246 ) ) ;
#15211 = ORIENTED_EDGE ( 'NONE', *, *, #3147, .T. ) ;
#15212 = VERTEX_POINT ( 'NONE', #6550 ) ;
#15213 = DIRECTION ( 'NONE',  ( 0.000000000000000000, 0.000000000000000000, -1.000000000000000000 ) ) ;
#15214 = AXIS2_PLACEMENT_3D ( 'NONE', #5338, #10663, #9294 ) ;
#15215 = CIRCLE ( 'NONE', #4780, 18.49999999999998934 ) ;
#15216 = APPLICATION_PROTOCOL_DEFINITION ( 'draft international standard', 'automotive_design', 1998, #9746 ) ;
#15217 = DIRECTION ( 'NONE',  ( 1.000000000000000000, 0.000000000000000000, 0.000000000000000000 ) ) ;
#15218 = CONICAL_SURFACE ( 'NONE', #15756, 13.89560290347679938, 1.567266246505109928 ) ;
#15219 = CYLINDRICAL_SURFACE ( 'NONE', #2724, 12.50000000000001066 ) ;
#15220 = VERTEX_POINT ( 'NONE', #10520 ) ;
#15221 = CARTESIAN_POINT ( 'NONE',  ( 0.000000000000000000, 16.00000000000000000, 0.000000000000000000 ) ) ;
#15222 = LINE ( 'NONE', #13757, #5594 ) ;
#15223 = PRODUCT_DEFINITION_FORMATION_WITH_SPECIFIED_SOURCE ( 'ANY', '', #13455, .NOT_KNOWN. ) ;
#15224 = EDGE_LOOP ( 'NONE', ( #1078, #15907, #1430, #13639 ) ) ;
#15225 = CARTESIAN_POINT ( 'NONE',  ( 30.99999999999997868, 0.000000000000000000, -30.99999999999999645 ) ) ;
#15226 = CARTESIAN_POINT ( 'NONE',  ( -37.00000000000000000, 68.00000000000000000, -22.99999999999999645 ) ) ;
#15227 = ORIENTED_EDGE ( 'NONE', *, *, #16022, .F. ) ;
#15228 = VECTOR ( 'NONE', #14237, 1000.000000000000000 ) ;
#15229 = DIRECTION ( 'NONE',  ( 0.000000000000000000, 0.000000000000000000, 1.000000000000000000 ) ) ;
#15230 = EDGE_CURVE ( 'NONE', #4587, #3093, #47, .T. ) ;
#15231 = VERTEX_POINT ( 'NONE', #2622 ) ;
#15232 = ORIENTED_EDGE ( 'NONE', *, *, #9729, .F. ) ;
#15233 = VERTEX_POINT ( 'NONE', #2279 ) ;
#15234 = EDGE_CURVE ( 'NONE', #13578, #2730, #7848, .T. ) ;
#15235 = ORIENTED_EDGE ( 'NONE', *, *, #1106, .T. ) ;
#15236 = ORIENTED_EDGE ( 'NONE', *, *, #9537, .F. ) ;
#15237 = CIRCLE ( 'NONE', #9211, 22.50000000000000000 ) ;
#15238 = DIRECTION ( 'NONE',  ( 0.000000000000000000, 1.000000000000000000, 0.000000000000000000 ) ) ;
#15239 = DIRECTION ( 'NONE',  ( -0.000000000000000000, -1.000000000000000000, 0.000000000000000000 ) ) ;
#15240 = CARTESIAN_POINT ( 'NONE',  ( -13.11912225705329327, 2.755455298081544778E-15, -22.50000000000000000 ) ) ;
#15241 = CYLINDRICAL_SURFACE ( 'NONE', #7466, 13.69540538389601991 ) ;
#15242 = CARTESIAN_POINT ( 'NONE',  ( -34.99999999999998579, 3.000000000000000000, 21.00000000000000355 ) ) ;
#15243 = PLANE ( 'NONE',  #5736 ) ;
#15244 = CARTESIAN_POINT ( 'NONE',  ( 45.00000000000000000, 559.9933750504617365, -546.7230258972048205 ) ) ;
#15245 = ORIENTED_EDGE ( 'NONE', *, *, #8022, .F. ) ;
#15246 = DIRECTION ( 'NONE',  ( 0.000000000000000000, -1.000000000000000000, 0.000000000000000000 ) ) ;
#15247 = FACE_OUTER_BOUND ( 'NONE', #8670, .T. ) ;
#15248 = ADVANCED_FACE ( 'NONE', ( #3665 ), #2361, .T. ) ;
#15249 = AXIS2_PLACEMENT_3D ( 'NONE', #14806, #13686, #16343 ) ;
#15250 = CIRCLE ( 'NONE', #4548, 3.299999999999997158 ) ;
#15251 = CYLINDRICAL_SURFACE ( 'NONE', #14817, 10.00000000000061995 ) ;
#15253 = ORIENTED_EDGE ( 'NONE', *, *, #9707, .F. ) ;
#15252 = EDGE_LOOP ( 'NONE', ( #10178, #5754 ) ) ;
#15254 = FACE_OUTER_BOUND ( 'NONE', #16346, .T. ) ;
#15255 = ORIENTED_EDGE ( 'NONE', *, *, #7721, .T. ) ;
#15256 = CARTESIAN_POINT ( 'NONE',  ( -31.81980515339462912, 8.000000000000000000, 28.51980515339464972 ) ) ;
#15257 = FACE_OUTER_BOUND ( 'NONE', #16264, .T. ) ;
#15258 = CARTESIAN_POINT ( 'NONE',  ( 54.99999999999999289, 515.4878487013597805, -546.7230258972048205 ) ) ;
#15259 = VECTOR ( 'NONE', #5301, 1000.000000000000000 ) ;
#15260 = ORIENTED_EDGE ( 'NONE', *, *, #8020, .F. ) ;
#15261 = ADVANCED_FACE ( 'NONE', ( #13108 ), #2441, .F. ) ;
#15262 = VECTOR ( 'NONE', #6756, 1000.000000000000000 ) ;
#15263 = CARTESIAN_POINT ( 'NONE',  ( 22.99999999999999645, 68.00000000000000000, 31.00000000000006750 ) ) ;
#15264 = LINE ( 'NONE', #13890, #473 ) ;
#15265 = ORIENTED_EDGE ( 'NONE', *, *, #6507, .F. ) ;
#15266 = DIRECTION ( 'NONE',  ( 0.000000000000000000, -1.000000000000000000, 0.000000000000000000 ) ) ;
#15267 = CARTESIAN_POINT ( 'NONE',  ( -20.99999999999999645, 8.000000000000000000, 35.00000000000001421 ) ) ;
#15268 = CARTESIAN_POINT ( 'NONE',  ( -31.81980515339462912, 11.00000000000000000, -31.81980515339465043 ) ) ;
#15269 = EDGE_CURVE ( 'NONE', #5852, #15724, #13022, .T. ) ;
#15270 = PLANE ( 'NONE',  #11110 ) ;
#15271 = DIRECTION ( 'NONE',  ( 1.000000000000000000, -0.000000000000000000, 0.000000000000000000 ) ) ;
#15272 = VERTEX_POINT ( 'NONE', #1510 ) ;
#15273 = AXIS2_PLACEMENT_3D ( 'NONE', #10697, #9250, #4272 ) ;
#15274 = DIRECTION ( 'NONE',  ( 0.000000000000000000, 0.000000000000000000, 1.000000000000000000 ) ) ;
#15275 = CIRCLE ( 'NONE', #7302, 84.99999999999997158 ) ;
#15276 = DIRECTION ( 'NONE',  ( -0.7327934916262990317, -0.6804510993672779895, -8.333122608164345406E-17 ) ) ;
#15277 = SHAPE_REPRESENTATION ( 'TAS-007', ( #5058, #2316, #11362, #3700, #14115, #8628, #13574, #6699, #2589, #15214, #5040, #16834, #11102, #11634 ), #13307 ) ;
#15278 = DIRECTION ( 'NONE',  ( 1.000000000000000000, 0.000000000000000000, -0.000000000000000000 ) ) ;
#15279 = EDGE_LOOP ( 'NONE', ( #9140, #10361, #2989, #2558 ) ) ;
#15280 = EDGE_CURVE ( 'NONE', #14137, #15298, #13282, .T. ) ;
#15281 = CARTESIAN_POINT ( 'NONE',  ( 44.68009836720079875, 380.0000000000000000, -17.00000000000000355 ) ) ;
#15282 = CIRCLE ( 'NONE', #7863, 3.300000000000004263 ) ;
#15283 = CARTESIAN_POINT ( 'NONE',  ( 0.000000000000000000, 341.5974953295086038, -15.94751227074151956 ) ) ;
#15284 = ORIENTED_EDGE ( 'NONE', *, *, #4380, .F. ) ;
#15285 = VECTOR ( 'NONE', #12890, 1000.000000000000000 ) ;
#15286 = FACE_OUTER_BOUND ( 'NONE', #11796, .T. ) ;
#15287 = EDGE_CURVE ( 'NONE', #8217, #1389, #311, .T. ) ;
#15288 = CARTESIAN_POINT ( 'NONE',  ( 0.000000000000000000, 449.3157724647197142, 33.76061909850716347 ) ) ;
#15289 = DIRECTION ( 'NONE',  ( -0.000000000000000000, -1.000000000000000000, -0.000000000000000000 ) ) ;
#15290 = VERTEX_POINT ( 'NONE', #4005 ) ;
#15291 = EDGE_CURVE ( 'NONE', #15586, #13772, #1675, .T. ) ;
#15292 = EDGE_CURVE ( 'NONE', #5130, #8924, #14821, .T. ) ;
#15293 = EDGE_CURVE ( 'NONE', #6651, #6319, #2879, .T. ) ;
#15294 = SURFACE_STYLE_USAGE ( .BOTH. , #4806 ) ;
#15295 = DIRECTION ( 'NONE',  ( 1.000000000000000000, 0.000000000000000000, 0.000000000000000000 ) ) ;
#15296 = CARTESIAN_POINT ( 'NONE',  ( -45.00000000000000000, 493.2350855268086320, -521.8755148539809170 ) ) ;
#15297 = VERTEX_POINT ( 'NONE', #14482 ) ;
#15298 = VERTEX_POINT ( 'NONE', #4349 ) ;
#15299 = DIRECTION ( 'NONE',  ( 0.000000000000000000, 0.000000000000000000, 1.000000000000000000 ) ) ;
#15300 = PRODUCT_CONTEXT ( 'NONE', #9746, 'mechanical' ) ;
#15301 =( LENGTH_UNIT ( ) NAMED_UNIT ( * ) SI_UNIT ( .MILLI., .METRE. ) );
#15302 = DIRECTION ( 'NONE',  ( 0.000000000000000000, -0.000000000000000000, -1.000000000000000000 ) ) ;
#15303 = ORIENTED_EDGE ( 'NONE', *, *, #12802, .T. ) ;
#15304 = CARTESIAN_POINT ( 'NONE',  ( -34.99999999999996447, 0.000000000000000000, -40.00000000000000711 ) ) ;
#15305 = FACE_OUTER_BOUND ( 'NONE', #2499, .T. ) ;
#15306 = ORIENTED_EDGE ( 'NONE', *, *, #12255, .T. ) ;
#15307 = LINE ( 'NONE', #6183, #12728 ) ;
#15308 = CARTESIAN_POINT ( 'NONE',  ( 21.00000000000000000, 19.00000000000000000, 35.00000000000001421 ) ) ;
#15309 = ORIENTED_EDGE ( 'NONE', *, *, #8448, .F. ) ;
#15310 = EDGE_CURVE ( 'NONE', #9087, #11776, #16016, .T. ) ;
#15311 = AXIS2_PLACEMENT_3D ( 'NONE', #1639, #6696, #190 ) ;
#15312 = FILL_AREA_STYLE_COLOUR ( '', #3674 ) ;
#15313 = ORIENTED_EDGE ( 'NONE', *, *, #8092, .F. ) ;
#15314 = VERTEX_POINT ( 'NONE', #10779 ) ;
#15315 = ORIENTED_EDGE ( 'NONE', *, *, #10761, .T. ) ;
#15316 = PRODUCT_DEFINITION_CONTEXT ( 'detailed design', #7630, 'design' ) ;
#15317 = ORIENTED_EDGE ( 'NONE', *, *, #12660, .F. ) ;
#15318 = ORIENTED_EDGE ( 'NONE', *, *, #3490, .F. ) ;
#15319 = LINE ( 'NONE', #9105, #13771 ) ;
#15320 = CIRCLE ( 'NONE', #7628, 4.999999999999997335 ) ;
#15321 = DIRECTION ( 'NONE',  ( 0.000000000000000000, 0.000000000000000000, 1.000000000000000000 ) ) ;
#15322 = CARTESIAN_POINT ( 'NONE',  ( 30.99999999999999645, 68.00000000000000000, 26.00000000000001066 ) ) ;
#15323 = CARTESIAN_POINT ( 'NONE',  ( 1.286622718088548112E-12, 258.6869404641209940, 288.5954239889852602 ) ) ;
#15324 = DIRECTION ( 'NONE',  ( 0.000000000000000000, 1.000000000000000000, 0.000000000000000000 ) ) ;
#15325 = DIRECTION ( 'NONE',  ( 0.000000000000000000, 0.000000000000000000, -1.000000000000000000 ) ) ;
#15326 = CARTESIAN_POINT ( 'NONE',  ( 1.163414457778310218E-15, 63.00000000000000000, 9.500000000000000000 ) ) ;
#15327 = PLANE ( 'NONE',  #4199 ) ;
#15328 = ORIENTED_EDGE ( 'NONE', *, *, #6870, .T. ) ;
#15329 = CARTESIAN_POINT ( 'NONE',  ( 0.000000000000000000, 620.7506394335853201, 0.000000000000000000 ) ) ;
#15330 = CARTESIAN_POINT ( 'NONE',  ( -2.216159785453297477E-13, 106.2500000000000142, 0.000000000000000000 ) ) ;
#15331 = AXIS2_PLACEMENT_3D ( 'NONE', #15244, #9767, #4666 ) ;
#15332 = PLANE ( 'NONE',  #14556 ) ;
#15334 = ORIENTED_EDGE ( 'NONE', *, *, #9600, .F. ) ;
#15333 = ORIENTED_EDGE ( 'NONE', *, *, #10334, .F. ) ;
#15335 = LINE ( 'NONE', #15415, #13606 ) ;
#15336 = ORIENTED_EDGE ( 'NONE', *, *, #15230, .T. ) ;
#15337 = VECTOR ( 'NONE', #10090, 1000.000000000000000 ) ;
#15338 = DIRECTION ( 'NONE',  ( -0.000000000000000000, -0.000000000000000000, 1.000000000000000000 ) ) ;
#15339 = DIRECTION ( 'NONE',  ( 1.000000000000000000, 0.000000000000000000, 0.000000000000000000 ) ) ;
#15340 = VERTEX_POINT ( 'NONE', #9581 ) ;
#15341 = PRODUCT_DEFINITION_SHAPE ( 'NONE', 'NONE',  #10102 ) ;
#15342 = UNCERTAINTY_MEASURE_WITH_UNIT (LENGTH_MEASURE( 1.000000000000000082E-05 ), #15168, 'distance_accuracy_value', 'NONE');
#15343 = CARTESIAN_POINT ( 'NONE',  ( -430.0000000000000568, 620.7506394335853201, 109.9999999999999858 ) ) ;
#15344 = DIRECTION ( 'NONE',  ( 0.000000000000000000, 0.000000000000000000, -1.000000000000000000 ) ) ;
#15345 = EDGE_LOOP ( 'NONE', ( #2943, #1274, #7453 ) ) ;
#15346 = CARTESIAN_POINT ( 'NONE',  ( -31.00000000000003197, 0.000000000000000000, -30.99999999999999289 ) ) ;
#15347 = DIRECTION ( 'NONE',  ( 0.000000000000000000, 0.000000000000000000, 1.000000000000000000 ) ) ;
#15348 = CARTESIAN_POINT ( 'NONE',  ( 46.99999999999988631, 473.6663340069158039, -566.6402177818052905 ) ) ;
#15349 = AXIS2_PLACEMENT_3D ( 'NONE', #4697, #12695, #4547 ) ;
#15350 = FACE_OUTER_BOUND ( 'NONE', #3454, .T. ) ;
#15351 = DIRECTION ( 'NONE',  ( 0.000000000000000000, 0.000000000000000000, -1.000000000000000000 ) ) ;
#15352 = ORIENTED_EDGE ( 'NONE', *, *, #22, .T. ) ;
#15353 = LINE ( 'NONE', #1264, #4812 ) ;
#15354 = EDGE_CURVE ( 'NONE', #11419, #7051, #5577, .T. ) ;
#15355 = FACE_OUTER_BOUND ( 'NONE', #3572, .T. ) ;
#15356 = CARTESIAN_POINT ( 'NONE',  ( -32.00000000000000711, 10.00000000000000000, -23.00000000000000000 ) ) ;
#15357 = EDGE_CURVE ( 'NONE', #16649, #11007, #3391, .T. ) ;
#15358 = CIRCLE ( 'NONE', #8220, 3.000000000000002665 ) ;
#15359 = ORIENTED_EDGE ( 'NONE', *, *, #8324, .T. ) ;
#15360 = AXIS2_PLACEMENT_3D ( 'NONE', #8311, #6674, #424 ) ;
#15361 = CARTESIAN_POINT ( 'NONE',  ( 21.99999999999998224, 8.000000000000000000, -35.99999999999999289 ) ) ;
#15362 = DIRECTION ( 'NONE',  ( -0.000000000000000000, 1.000000000000000000, -0.000000000000000000 ) ) ;
#15363 = ORIENTED_EDGE ( 'NONE', *, *, #16865, .F. ) ;
#15364 = DIRECTION ( 'NONE',  ( 0.000000000000000000, 1.000000000000000000, 0.000000000000000000 ) ) ;
#15365 = DIRECTION ( 'NONE',  ( 0.000000000000000000, 0.000000000000000000, -1.000000000000000000 ) ) ;
#15366 = LINE ( 'NONE', #13918, #1818 ) ;
#15367 = VERTEX_POINT ( 'NONE', #11988 ) ;
#15368 = CARTESIAN_POINT ( 'NONE',  ( -33.00000000000000000, 10.00000000000000000, -22.00000000000000355 ) ) ;
#15369 = DIRECTION ( 'NONE',  ( 1.000000000000000000, -0.000000000000000000, 0.000000000000000000 ) ) ;
#15370 = DIRECTION ( 'NONE',  ( 1.000000000000000000, 0.000000000000000000, 0.000000000000000000 ) ) ;
#15371 = ORIENTED_EDGE ( 'NONE', *, *, #9738, .T. ) ;
#15372 = VECTOR ( 'NONE', #10510, 1000.000000000000000 ) ;
#15373 = DIRECTION ( 'NONE',  ( 1.000000000000000000, -0.000000000000000000, 0.000000000000000000 ) ) ;
#15374 = EDGE_CURVE ( 'NONE', #7984, #3758, #10692, .T. ) ;
#15375 = VECTOR ( 'NONE', #4919, 1000.000000000000000 ) ;
#15376 = ITEM_DEFINED_TRANSFORMATION ( 'NONE', 'NONE', #11634,  #1780 ) ;
#15377 = EDGE_CURVE ( 'NONE', #11680, #13507, #8021, .T. ) ;
#15378 = DIRECTION ( 'NONE',  ( -0.000000000000000000, -1.000000000000000000, -0.000000000000000000 ) ) ;
#15379 = ADVANCED_FACE ( 'NONE', ( #14739, #1772 ), #5446, .T. ) ;
#15380 = EDGE_LOOP ( 'NONE', ( #12732, #11181, #2716, #15484 ) ) ;
#15381 = ADVANCED_FACE ( 'NONE', ( #2965 ), #2848, .T. ) ;
#15382 = CARTESIAN_POINT ( 'NONE',  ( -55.99999999999989342, 559.9933750504617365, -546.7230258972048205 ) ) ;
#15383 = LINE ( 'NONE', #4899, #3957 ) ;
#15384 = AXIS2_PLACEMENT_3D ( 'NONE', #6665, #158, #13304 ) ;
#15385 = ORIENTED_EDGE ( 'NONE', *, *, #5235, .F. ) ;
#15386 = DIRECTION ( 'NONE',  ( 0.000000000000000000, 0.000000000000000000, 1.000000000000000000 ) ) ;
#15387 = DIRECTION ( 'NONE',  ( 0.000000000000000000, 1.000000000000000000, 1.321694076934710402E-16 ) ) ;
#15388 = EDGE_LOOP ( 'NONE', ( #7817, #14267, #2863, #1055 ) ) ;
#15389 = CARTESIAN_POINT ( 'NONE',  ( 2.999999999999996891, 60.00000000000000711, 6.000000000000000000 ) ) ;
#15390 = EDGE_LOOP ( 'NONE', ( #15189, #8357, #1404, #274 ) ) ;
#15391 = EDGE_LOOP ( 'NONE', ( #9118, #7794, #9713, #10495 ) ) ;
#15392 = ORIENTED_EDGE ( 'NONE', *, *, #3946, .F. ) ;
#15393 = VECTOR ( 'NONE', #12652, 1000.000000000000000 ) ;
#15394 = ORIENTED_EDGE ( 'NONE', *, *, #4859, .F. ) ;
#15395 = ADVANCED_FACE ( 'NONE', ( #13538 ), #15187, .T. ) ;
#15396 = EDGE_CURVE ( 'NONE', #6601, #16595, #16014, .T. ) ;
#15397 = ORIENTED_EDGE ( 'NONE', *, *, #1958, .F. ) ;
#15398 = EDGE_CURVE ( 'NONE', #9815, #1644, #111, .T. ) ;
#15399 = CARTESIAN_POINT ( 'NONE',  ( 0.000000000000000000, 339.1725919290084335, -104.9456657433597968 ) ) ;
#15400 = CARTESIAN_POINT ( 'NONE',  ( 30.99999999999997513, 10.00000000000000000, 25.99999999999999645 ) ) ;
#15401 = PLANE ( 'NONE',  #9834 ) ;
#15402 = LINE ( 'NONE', #7483, #13802 ) ;
#15403 = DIRECTION ( 'NONE',  ( -6.123031769111888756E-17, 1.000000000000000000, 3.749151804555344967E-33 ) ) ;
#15404 = CIRCLE ( 'NONE', #14314, 3.999999999999996447 ) ;
#15405 = CARTESIAN_POINT ( 'NONE',  ( -149.9999999999998579, -3.835054598945682812E-14, 0.000000000000000000 ) ) ;
#15406 = FACE_OUTER_BOUND ( 'NONE', #11612, .T. ) ;
#15407 = ORIENTED_EDGE ( 'NONE', *, *, #16934, .T. ) ;
#15408 = DIRECTION ( 'NONE',  ( 1.000000000000000000, 0.000000000000000000, -0.000000000000000000 ) ) ;
#15409 = DIRECTION ( 'NONE',  ( -0.000000000000000000, 0.000000000000000000, 1.000000000000000000 ) ) ;
#15410 = ORIENTED_EDGE ( 'NONE', *, *, #10669, .F. ) ;
#15411 = AXIS2_PLACEMENT_3D ( 'NONE', #1541, #6934, #5658 ) ;
#15412 = LINE ( 'NONE', #10268, #5769 ) ;
#15414 = ORIENTED_EDGE ( 'NONE', *, *, #5916, .F. ) ;
#15413 = EDGE_LOOP ( 'NONE', ( #1246, #16906, #368, #3359, #1571, #10328, #5954, #13129 ) ) ;
#15415 = CARTESIAN_POINT ( 'NONE',  ( 449.9999999999998295, 135.5000000000000000, 3.000000000000000000 ) ) ;
#15416 = ORIENTED_EDGE ( 'NONE', *, *, #1703, .T. ) ;
#15417 = VECTOR ( 'NONE', #16740, 1000.000000000000000 ) ;
#15418 = DIRECTION ( 'NONE',  ( 1.000000000000000000, 0.000000000000000000, -0.000000000000000000 ) ) ;
#15419 = FACE_OUTER_BOUND ( 'NONE', #5801, .T. ) ;
#15420 = CARTESIAN_POINT ( 'NONE',  ( -18.00000000000000711, 6.452029775889750974E-16, 5.268482129199949959 ) ) ;
#15421 = CIRCLE ( 'NONE', #1236, 20.75209553982837463 ) ;
#15422 = ORIENTED_EDGE ( 'NONE', *, *, #7802, .T. ) ;
#15423 = CIRCLE ( 'NONE', #8009, 13.69540538389601991 ) ;
#15424 = AXIS2_PLACEMENT_3D ( 'NONE', #15058, #7143, #8281 ) ;
#15425 = CARTESIAN_POINT ( 'NONE',  ( -31.00000000000007105, 0.000000000000000000, 23.00000000000000000 ) ) ;
#15426 = DIRECTION ( 'NONE',  ( 0.000000000000000000, 0.000000000000000000, 1.000000000000000000 ) ) ;
#15427 = ORIENTED_EDGE ( 'NONE', *, *, #6634, .F. ) ;
#15428 = CARTESIAN_POINT ( 'NONE',  ( 45.00000000000000000, 523.2161522479893847, -576.8570079137933817 ) ) ;
#15429 = PLANE ( 'NONE',  #15803 ) ;
#15430 = DIRECTION ( 'NONE',  ( -1.000000000000000000, 0.000000000000000000, 0.000000000000000000 ) ) ;
#15431 = AXIS2_PLACEMENT_3D ( 'NONE', #248, #3936, #14681 ) ;
#15432 = LINE ( 'NONE', #10291, #3960 ) ;
#15433 = CARTESIAN_POINT ( 'NONE',  ( -2.216159785453297477E-13, 104.2500000000000142, 0.000000000000000000 ) ) ;
#15434 = ORIENTED_EDGE ( 'NONE', *, *, #2246, .F. ) ;
#15435 = CARTESIAN_POINT ( 'NONE',  ( -26.00000000000000355, 19.00000000000000000, 31.00000000000003197 ) ) ;
#15436 = VECTOR ( 'NONE', #3156, 1000.000000000000000 ) ;
#15437 = VECTOR ( 'NONE', #6486, 1000.000000000000000 ) ;
#15438 = ADVANCED_FACE ( 'NONE', ( #4086 ), #9323, .F. ) ;
#15439 = CARTESIAN_POINT ( 'NONE',  ( 394.0000000000001137, 341.5974953295086038, -15.94751227074151956 ) ) ;
#15440 = LINE ( 'NONE', #3769, #1165 ) ;
#15441 = VECTOR ( 'NONE', #12656, 1000.000000000000000 ) ;
#15442 = EDGE_LOOP ( 'NONE', ( #16719, #6893, #3402, #10076 ) ) ;
#15443 = CARTESIAN_POINT ( 'NONE',  ( 0.000000000000000000, 306.0487089519837127, -150.0000000000038369 ) ) ;
#15444 = AXIS2_PLACEMENT_3D ( 'NONE', #3991, #2427, #1146 ) ;
#15445 = VECTOR ( 'NONE', #12029, 1000.000000000000000 ) ;
#15446 = PRODUCT_RELATED_PRODUCT_CATEGORY ( 'part', '', ( #9040 ) ) ;
#15447 = DIRECTION ( 'NONE',  ( 6.123031769111888756E-17, -1.000000000000000000, -3.749151804555344967E-33 ) ) ;
#15448 = VERTEX_POINT ( 'NONE', #13864 ) ;
#15449 = DIRECTION ( 'NONE',  ( 0.000000000000000000, 0.000000000000000000, 1.000000000000000000 ) ) ;
#15450 = AXIS2_PLACEMENT_3D ( 'NONE', #6722, #13356, #9233 ) ;
#15451 = VECTOR ( 'NONE', #11642, 1000.000000000000000 ) ;
#15452 = DIRECTION ( 'NONE',  ( 1.000000000000000000, 0.000000000000000000, 0.000000000000000000 ) ) ;
#15453 = CARTESIAN_POINT ( 'NONE',  ( 10.00000000000000000, 620.7506394335853201, -11.00000000000000000 ) ) ;
#15454 = ORIENTED_EDGE ( 'NONE', *, *, #2697, .T. ) ;
#15455 = LINE ( 'NONE', #9018, #9541 ) ;
#15456 = DIRECTION ( 'NONE',  ( -0.000000000000000000, 0.000000000000000000, -1.000000000000000000 ) ) ;
#15457 = EDGE_LOOP ( 'NONE', ( #16490, #5202, #2510, #11949 ) ) ;
#15458 = AXIS2_PLACEMENT_3D ( 'NONE', #6260, #15558, #6512 ) ;
#15459 = EDGE_CURVE ( 'NONE', #15233, #9156, #8617, .T. ) ;
#15460 = FACE_OUTER_BOUND ( 'NONE', #10219, .T. ) ;
#15461 = AXIS2_PLACEMENT_3D ( 'NONE', #12640, #7388, #9901 ) ;
#15462 = VECTOR ( 'NONE', #16108, 1000.000000000000227 ) ;
#15463 = CIRCLE ( 'NONE', #10798, 4.999999999999997335 ) ;
#15464 = ORIENTED_EDGE ( 'NONE', *, *, #3328, .T. ) ;
#15465 = AXIS2_PLACEMENT_3D ( 'NONE', #8293, #2974, #16446 ) ;
#15466 = CARTESIAN_POINT ( 'NONE',  ( 46.99999999999988631, 549.5810598491746077, -522.8108303813202156 ) ) ;
#15467 = DIRECTION ( 'NONE',  ( 1.000000000000000000, 0.000000000000000000, 0.000000000000000000 ) ) ;
#15468 = CIRCLE ( 'NONE', #7230, 12.50000000000001066 ) ;
#15469 = EDGE_CURVE ( 'NONE', #1233, #12242, #12491, .T. ) ;
#15470 = DIRECTION ( 'NONE',  ( 0.000000000000000000, -0.000000000000000000, 1.000000000000000000 ) ) ;
#15471 = VERTEX_POINT ( 'NONE', #1850 ) ;
#15472 = DIRECTION ( 'NONE',  ( 0.9998870921963913805, 0.01502673813723916056, -0.000000000000000000 ) ) ;
#15473 = FACE_OUTER_BOUND ( 'NONE', #14870, .T. ) ;
#15474 = ORIENTED_EDGE ( 'NONE', *, *, #10766, .F. ) ;
#15475 = VECTOR ( 'NONE', #2139, 1000.000000000000000 ) ;
#15476 = CARTESIAN_POINT ( 'NONE',  ( -26.00000000000001776, 8.000000000000000000, 33.00000000000000711 ) ) ;
#15477 = CIRCLE ( 'NONE', #9992, 4.695405383896011919 ) ;
#15478 = ORIENTED_EDGE ( 'NONE', *, *, #245, .F. ) ;
#15479 = EDGE_CURVE ( 'NONE', #2730, #16527, #1203, .T. ) ;
#15480 = VERTEX_POINT ( 'NONE', #16514 ) ;
#15481 = EDGE_CURVE ( 'NONE', #14388, #12590, #10809, .T. ) ;
#15482 = PLANE ( 'NONE',  #8635 ) ;
#15483 = VECTOR ( 'NONE', #11005, 1000.000000000000000 ) ;
#15484 = ORIENTED_EDGE ( 'NONE', *, *, #11099, .F. ) ;
#15485 = CARTESIAN_POINT ( 'NONE',  ( 527.1139154823663375, 313.4055085939265837, -202.0530008001410067 ) ) ;
#15486 = ORIENTED_EDGE ( 'NONE', *, *, #2457, .T. ) ;
#15487 = VERTEX_POINT ( 'NONE', #892 ) ;
#15488 =( GEOMETRIC_REPRESENTATION_CONTEXT ( 3 ) GLOBAL_UNCERTAINTY_ASSIGNED_CONTEXT ( ( #5321 ) ) GLOBAL_UNIT_ASSIGNED_CONTEXT ( ( #15914, #1588, #6889 ) ) REPRESENTATION_CONTEXT ( 'NONE', 'WORKASPACE' ) );
#15489 = DIRECTION ( 'NONE',  ( 1.000000000000000000, 0.000000000000000000, -0.000000000000000000 ) ) ;
#15490 = CARTESIAN_POINT ( 'NONE',  ( 54.99999999999999289, 515.4878487013597805, -546.7230258972048205 ) ) ;
#15491 = ADVANCED_FACE ( 'NONE', ( #4513 ), #16432, .T. ) ;
#15492 = ORIENTED_EDGE ( 'NONE', *, *, #12126, .T. ) ;
#15493 = AXIS2_PLACEMENT_3D ( 'NONE', #10640, #15873, #4112 ) ;
#15494 = FACE_OUTER_BOUND ( 'NONE', #16009, .T. ) ;
#15495 = EDGE_CURVE ( 'NONE', #1294, #1641, #6031, .T. ) ;
#15496 = CARTESIAN_POINT ( 'NONE',  ( -8.636442107178585067E-13, 290.3130897954760030, 29.03130897954724787 ) ) ;
#15497 = FACE_OUTER_BOUND ( 'NONE', #16930, .T. ) ;
#15498 = CYLINDRICAL_SURFACE ( 'NONE', #6941, 10.00000000000000178 ) ;
#15499 = EDGE_CURVE ( 'NONE', #6145, #2977, #2092, .T. ) ;
#15500 = ORIENTED_EDGE ( 'NONE', *, *, #10367, .F. ) ;
#15501 = DIRECTION ( 'NONE',  ( -0.000000000000000000, -1.000000000000000000, -0.000000000000000000 ) ) ;
#15502 = DIRECTION ( 'NONE',  ( 0.000000000000000000, 1.000000000000000000, 0.000000000000000000 ) ) ;
#15503 = ORIENTED_EDGE ( 'NONE', *, *, #8416, .F. ) ;
#15504 = EDGE_CURVE ( 'NONE', #10620, #2369, #15463, .T. ) ;
#15505 = EDGE_CURVE ( 'NONE', #11290, #11248, #4590, .T. ) ;
#15506 = EDGE_CURVE ( 'NONE', #16566, #5055, #2560, .T. ) ;
#15507 = FACE_OUTER_BOUND ( 'NONE', #9807, .T. ) ;
#15509 = EDGE_LOOP ( 'NONE', ( #7796, #13230, #16621, #2408 ) ) ;
#15508 = VERTEX_POINT ( 'NONE', #7323 ) ;
#15510 = CARTESIAN_POINT ( 'NONE',  ( -46.99999999999988631, 523.2161522479893847, -604.2478186815853860 ) ) ;
#15511 = CIRCLE ( 'NONE', #1805, 3.299999999999997158 ) ;
#15512 = ORIENTED_EDGE ( 'NONE', *, *, #7068, .F. ) ;
#15513 = ORIENTED_EDGE ( 'NONE', *, *, #4003, .F. ) ;
#15514 = CARTESIAN_POINT ( 'NONE',  ( 10.00000000000000000, 372.8685141053778693, -86.48019484660871115 ) ) ;
#15515 = CARTESIAN_POINT ( 'NONE',  ( 7.000000000000001776, 0.000000000000000000, -65.00000000000000000 ) ) ;
#15516 = CARTESIAN_POINT ( 'NONE',  ( 39.41161623800082481, 323.9612906317821057, -6.736600000000000144 ) ) ;
#15517 = ORIENTED_EDGE ( 'NONE', *, *, #5725, .T. ) ;
#15518 = CARTESIAN_POINT ( 'NONE',  ( -55.99999999999989342, 523.2161522479888163, -502.8936384967199729 ) ) ;
#15519 = ORIENTED_EDGE ( 'NONE', *, *, #10847, .F. ) ;
#15520 = DIRECTION ( 'NONE',  ( -0.000000000000000000, 1.000000000000000000, -0.000000000000000000 ) ) ;
#15521 = VECTOR ( 'NONE', #2274, 1000.000000000000000 ) ;
#15522 = DIRECTION ( 'NONE',  ( -1.000000000000000000, -0.000000000000000000, -0.000000000000000000 ) ) ;
#15523 = CARTESIAN_POINT ( 'NONE',  ( -26.00000000000002132, 10.00000000000000000, -39.99999999999999289 ) ) ;
#15524 = EDGE_CURVE ( 'NONE', #2162, #10866, #14902, .T. ) ;
#15525 = DIRECTION ( 'NONE',  ( -0.000000000000000000, -1.000000000000000000, -0.000000000000000000 ) ) ;
#15526 = CYLINDRICAL_SURFACE ( 'NONE', #6833, 13.69540538389601991 ) ;
#15527 = ADVANCED_BREP_SHAPE_REPRESENTATION ( '', ( #8514, #1488 ), #8346 ) ;
#15528 = ORIENTED_EDGE ( 'NONE', *, *, #15481, .F. ) ;
#15529 = CARTESIAN_POINT ( 'NONE',  ( 31.00000000000000000, 11.00000000000000000, 30.99999999999999289 ) ) ;
#15530 = AXIS2_PLACEMENT_3D ( 'NONE', #4884, #3353, #610 ) ;
#15531 = DIRECTION ( 'NONE',  ( 1.000000000000000000, 0.000000000000000000, 0.000000000000000000 ) ) ;
#15532 = VECTOR ( 'NONE', #13990, 1000.000000000000000 ) ;
#15533 = CARTESIAN_POINT ( 'NONE',  ( -46.99999999999988631, 523.2161522479888163, -502.8936384967199729 ) ) ;
#15534 = ORIENTED_EDGE ( 'NONE', *, *, #11377, .T. ) ;
#15535 = CARTESIAN_POINT ( 'NONE',  ( 56.73000000000001108, 261.2094592450224582, 287.2045212030221251 ) ) ;
#15536 = CARTESIAN_POINT ( 'NONE',  ( -21.00000000000002842, 0.000000000000000000, -37.50000000000000000 ) ) ;
#15537 = ORIENTED_EDGE ( 'NONE', *, *, #12250, .T. ) ;
#15538 = CARTESIAN_POINT ( 'NONE',  ( -6.117449311278464482E-17, 277.8092731128509740, -29.71049682360898103 ) ) ;
#15539 = DIRECTION ( 'NONE',  ( 0.000000000000000000, 0.9271838545667883125, 0.3746065934159094613 ) ) ;
#15540 = CARTESIAN_POINT ( 'NONE',  ( -22.99999999999999645, 0.000000000000000000, -31.00000000000005684 ) ) ;
#15541 = CARTESIAN_POINT ( 'NONE',  ( 394.0000000000001137, 234.3157724647196289, -104.2090657433598011 ) ) ;
#15542 = CIRCLE ( 'NONE', #11152, 18.50000000000000000 ) ;
#15543 = VECTOR ( 'NONE', #12682, 1000.000000000000000 ) ;
#15544 = LINE ( 'NONE', #9094, #12352 ) ;
#15545 = FACE_OUTER_BOUND ( 'NONE', #16423, .T. ) ;
#15546 = DIRECTION ( 'NONE',  ( -1.000000000000000000, -0.000000000000000000, -0.000000000000000000 ) ) ;
#15547 = ORIENTED_EDGE ( 'NONE', *, *, #13927, .F. ) ;
#15548 = FACE_OUTER_BOUND ( 'NONE', #4339, .T. ) ;
#15549 = APPLICATION_CONTEXT ( 'automotive_design' ) ;
#15550 = DIRECTION ( 'NONE',  ( -1.000000000000000000, 2.952167314869161697E-31, 6.982962677686267499E-15 ) ) ;
#15551 = CIRCLE ( 'NONE', #3766, 13.69540538389601991 ) ;
#15552 = VERTEX_POINT ( 'NONE', #12323 ) ;
#15553 = VECTOR ( 'NONE', #6514, 1000.000000000000000 ) ;
#15554 = LINE ( 'NONE', #3867, #1156 ) ;
#15555 = DIRECTION ( 'NONE',  ( 1.000000000000000000, 0.000000000000000000, 0.000000000000000000 ) ) ;
#15556 = CARTESIAN_POINT ( 'NONE',  ( 0.000000000000000000, 372.8685141053783241, -146.8198051533979935 ) ) ;
#15557 = ORIENTED_EDGE ( 'NONE', *, *, #13582, .T. ) ;
#15558 = DIRECTION ( 'NONE',  ( 1.000000000000000000, -0.000000000000000000, 0.000000000000000000 ) ) ;
#15559 = CARTESIAN_POINT ( 'NONE',  ( 21.00000000000000000, 8.000000000000000000, 35.00000000000001421 ) ) ;
#15560 = ORIENTED_EDGE ( 'NONE', *, *, #7274, .F. ) ;
#15561 = PLANE ( 'NONE',  #1202 ) ;
#15562 = VERTEX_POINT ( 'NONE', #13625 ) ;
#15563 = ORIENTED_EDGE ( 'NONE', *, *, #7691, .T. ) ;
#15564 = AXIS2_PLACEMENT_3D ( 'NONE', #8151, #5657, #4202 ) ;
#15565 = LINE ( 'NONE', #5153, #1209 ) ;
#15566 = ORIENTED_EDGE ( 'NONE', *, *, #12151, .T. ) ;
#15567 = EDGE_CURVE ( 'NONE', #8690, #14019, #5789, .T. ) ;
#15568 = ORIENTED_EDGE ( 'NONE', *, *, #9413, .T. ) ;
#15569 = VERTEX_POINT ( 'NONE', #14991 ) ;
#15570 = CYLINDRICAL_SURFACE ( 'NONE', #13506, 13.69540538389601991 ) ;
#15571 = DIRECTION ( 'NONE',  ( 1.000000000000000000, 0.000000000000000000, 0.000000000000000000 ) ) ;
#15572 = AXIS2_PLACEMENT_3D ( 'NONE', #1622, #5566, #5738 ) ;
#15573 = ADVANCED_FACE ( 'NONE', ( #814 ), #3227, .F. ) ;
#15574 = ORIENTED_EDGE ( 'NONE', *, *, #14644, .F. ) ;
#15575 = DIRECTION ( 'NONE',  ( 0.000000000000000000, 0.000000000000000000, 1.000000000000000000 ) ) ;
#15576 = DIRECTION ( 'NONE',  ( 0.000000000000000000, 1.000000000000000000, 0.000000000000000000 ) ) ;
#15577 = VERTEX_POINT ( 'NONE', #12403 ) ;
#15578 = CARTESIAN_POINT ( 'NONE',  ( 0.000000000000000000, -3.000000000000000000, 0.000000000000000000 ) ) ;
#15579 = ORIENTED_EDGE ( 'NONE', *, *, #7725, .F. ) ;
#15580 = CARTESIAN_POINT ( 'NONE',  ( 45.00000000000000000, 515.4878487013597805, -606.7230258972047068 ) ) ;
#15581 = ORIENTED_EDGE ( 'NONE', *, *, #13399, .T. ) ;
#15582 = DIRECTION ( 'NONE',  ( -0.000000000000000000, -0.000000000000000000, -1.000000000000000000 ) ) ;
#15583 = ADVANCED_FACE ( 'NONE', ( #641 ), #5876, .T. ) ;
#15584 = AXIS2_PLACEMENT_3D ( 'NONE', #13419, #13148, #356 ) ;
#15585 = ORIENTED_EDGE ( 'NONE', *, *, #15158, .F. ) ;
#15586 = VERTEX_POINT ( 'NONE', #13776 ) ;
#15587 = FILL_AREA_STYLE_COLOUR ( '', #11027 ) ;
#15588 = DIRECTION ( 'NONE',  ( -0.000000000000000000, -1.000000000000000000, 0.000000000000000000 ) ) ;
#15589 = EDGE_CURVE ( 'NONE', #4239, #12007, #2004, .T. ) ;
#15590 = DIRECTION ( 'NONE',  ( -0.000000000000000000, -1.000000000000000000, -0.000000000000000000 ) ) ;
#15591 = EDGE_CURVE ( 'NONE', #15631, #9007, #5958, .T. ) ;
#15593 = ORIENTED_EDGE ( 'NONE', *, *, #5354, .T. ) ;
#15592 = EDGE_CURVE ( 'NONE', #5349, #3811, #16853, .T. ) ;
#15595 = ADVANCED_FACE ( 'NONE', ( #979 ), #6113, .F. ) ;
#15594 = DIRECTION ( 'NONE',  ( 1.000000000000000000, 0.000000000000000000, 0.000000000000000000 ) ) ;
#15596 = DIRECTION ( 'NONE',  ( 0.000000000000000000, -0.000000000000000000, 1.000000000000000000 ) ) ;
#15597 = CYLINDRICAL_SURFACE ( 'NONE', #14539, 22.75209553982837463 ) ;
#15598 = CIRCLE ( 'NONE', #3531, 4.999999999999997335 ) ;
#15599 = CARTESIAN_POINT ( 'NONE',  ( 0.3042215205882442541, 192.9067263765842881, 37.35332311086163060 ) ) ;
#15600 = CARTESIAN_POINT ( 'NONE',  ( 55.99999999999989342, 559.9933750504617365, -546.7230258972048205 ) ) ;
#15601 = PLANE ( 'NONE',  #9471 ) ;
#15602 = DIRECTION ( 'NONE',  ( 1.000000000000000000, -0.000000000000000000, 0.000000000000000000 ) ) ;
#15604 = VERTEX_POINT ( 'NONE', #15400 ) ;
#15603 = VERTEX_POINT ( 'NONE', #7736 ) ;
#15605 = DIRECTION ( 'NONE',  ( -0.000000000000000000, 1.000000000000000000, -8.952264470854156086E-17 ) ) ;
#15606 = CARTESIAN_POINT ( 'NONE',  ( 40.00000000000000711, 11.00000000000000000, -34.99999999999997868 ) ) ;
#15607 = EDGE_CURVE ( 'NONE', #4673, #6723, #11366, .T. ) ;
#15608 = DIRECTION ( 'NONE',  ( -1.000000000000000000, 0.000000000000000000, -0.000000000000000000 ) ) ;
#15609 = EDGE_CURVE ( 'NONE', #14192, #4223, #6195, .T. ) ;
#15610 = ORIENTED_EDGE ( 'NONE', *, *, #6811, .F. ) ;
#15611 = EDGE_CURVE ( 'NONE', #974, #11696, #8329, .T. ) ;
#15612 = DIRECTION ( 'NONE',  ( 0.000000000000000000, 0.000000000000000000, -1.000000000000000000 ) ) ;
#15613 = CIRCLE ( 'NONE', #4645, 8.000000000000000000 ) ;
#15614 = DIRECTION ( 'NONE',  ( 0.000000000000000000, 1.000000000000000000, 0.000000000000000000 ) ) ;
#15615 = ORIENTED_EDGE ( 'NONE', *, *, #9293, .F. ) ;
#15616 = CARTESIAN_POINT ( 'NONE',  ( -23.00000000000002487, 10.00000000000000000, -36.99999999999999289 ) ) ;
#15617 = LINE ( 'NONE', #2308, #5159 ) ;
#15618 = CYLINDRICAL_SURFACE ( 'NONE', #14713, 187.4999999999998863 ) ;
#15619 = ORIENTED_EDGE ( 'NONE', *, *, #10246, .F. ) ;
#15620 = CARTESIAN_POINT ( 'NONE',  ( -34.99999999999996447, 8.000000000000000000, 40.00000000000000711 ) ) ;
#15621 =( NAMED_UNIT ( * ) SI_UNIT ( $, .STERADIAN. ) SOLID_ANGLE_UNIT ( ) );
#15622 = CARTESIAN_POINT ( 'NONE',  ( 0.7365999999999761627, 286.2094592450219466, 37.20452120302238086 ) ) ;
#15623 = EDGE_LOOP ( 'NONE', ( #7646, #9904 ) ) ;
#15624 = EDGE_CURVE ( 'NONE', #13859, #903, #12904, .T. ) ;
#15625 = VECTOR ( 'NONE', #13876, 1000.000000000000114 ) ;
#15626 = DIRECTION ( 'NONE',  ( 1.000000000000000000, 0.000000000000000000, 0.000000000000000000 ) ) ;
#15627 = ORIENTED_EDGE ( 'NONE', *, *, #3213, .T. ) ;
#15628 = DIRECTION ( 'NONE',  ( -0.000000000000000000, -1.000000000000000000, -0.000000000000000000 ) ) ;
#15629 = PLANE ( 'NONE',  #12466 ) ;
#15630 = CARTESIAN_POINT ( 'NONE',  ( 1.469576158976824144E-15, 0.000000000000000000, 12.00000000000000178 ) ) ;
#15631 = VERTEX_POINT ( 'NONE', #2252 ) ;
#15632 = DIRECTION ( 'NONE',  ( 0.000000000000000000, 1.000000000000000000, 0.000000000000000000 ) ) ;
#15633 = CARTESIAN_POINT ( 'NONE',  ( 21.99999999999998224, 10.00000000000000000, -35.99999999999999289 ) ) ;
#15634 = ORIENTED_EDGE ( 'NONE', *, *, #5247, .T. ) ;
#15635 = AXIS2_PLACEMENT_3D ( 'NONE', #7926, #15836, #1500 ) ;
#15636 = CIRCLE ( 'NONE', #15360, 15.14120580695350071 ) ;
#15637 = DIRECTION ( 'NONE',  ( -0.000000000000000000, -1.000000000000000000, -0.000000000000000000 ) ) ;
#15638 = ORIENTED_EDGE ( 'NONE', *, *, #9203, .T. ) ;
#15639 = ORIENTED_EDGE ( 'NONE', *, *, #287, .T. ) ;
#15640 = LINE ( 'NONE', #7818, #10261 ) ;
#15641 = EDGE_LOOP ( 'NONE', ( #1064, #6955, #3373, #8001 ) ) ;
#15642 = CARTESIAN_POINT ( 'NONE',  ( 415.0210210471910841, 329.6061121441327941, 10.00000000000000178 ) ) ;
#15643 = ORIENTED_EDGE ( 'NONE', *, *, #16948, .F. ) ;
#15644 = VERTEX_POINT ( 'NONE', #3556 ) ;
#15645 = CARTESIAN_POINT ( 'NONE',  ( 55.99999999999989342, 473.6663340069157471, -531.5012393965008641 ) ) ;
#15646 = DIRECTION ( 'NONE',  ( 0.000000000000000000, 0.000000000000000000, 1.000000000000000000 ) ) ;
#15647 = VERTEX_POINT ( 'NONE', #8963 ) ;
#15648 = CARTESIAN_POINT ( 'NONE',  ( 414.7091847417151484, 350.3558646104334571, 0.000000000000000000 ) ) ;
#15649 = EDGE_CURVE ( 'NONE', #15290, #5055, #4836, .T. ) ;
#15650 = CARTESIAN_POINT ( 'NONE',  ( 394.0000000000001137, 339.1725919290087745, -16.41886574335978821 ) ) ;
#15651 = ORIENTED_EDGE ( 'NONE', *, *, #9959, .T. ) ;
#15652 = FACE_BOUND ( 'NONE', #2240, .T. ) ;
#15653 = CARTESIAN_POINT ( 'NONE',  ( -37.00000000000000711, 6.000000000000000000, 23.00000000000000000 ) ) ;
#15654 = ORIENTED_EDGE ( 'NONE', *, *, #12363, .F. ) ;
#15655 = VECTOR ( 'NONE', #2964, 1000.000000000000000 ) ;
#15656 = CARTESIAN_POINT ( 'NONE',  ( 25.99999999999996092, 3.000000000000000000, 31.00000000000004263 ) ) ;
#15657 = ORIENTED_EDGE ( 'NONE', *, *, #8125, .F. ) ;
#15658 = ADVANCED_FACE ( 'NONE', ( #11615 ), #4499, .T. ) ;
#15659 = DIRECTION ( 'NONE',  ( 0.000000000000000000, 1.000000000000000000, 0.000000000000000000 ) ) ;
#15660 = ORIENTED_EDGE ( 'NONE', *, *, #4062, .T. ) ;
#15661 = VERTEX_POINT ( 'NONE', #11448 ) ;
#15662 = CARTESIAN_POINT ( 'NONE',  ( 30.99999999999995737, 3.000000000000000000, 31.00000000000000000 ) ) ;
#15663 = CARTESIAN_POINT ( 'NONE',  ( -430.0000000000000568, 425.7506394335853201, 0.000000000000000000 ) ) ;
#15664 = DIRECTION ( 'NONE',  ( 0.000000000000000000, 0.000000000000000000, -1.000000000000000000 ) ) ;
#15665 = CIRCLE ( 'NONE', #9106, 7.999999999999996447 ) ;
#15666 = ORIENTED_EDGE ( 'NONE', *, *, #8143, .F. ) ;
#15667 = CARTESIAN_POINT ( 'NONE',  ( -31.00000000000006395, 3.000000000000000000, -25.99999999999999645 ) ) ;
#15668 = DIRECTION ( 'NONE',  ( 0.000000000000000000, -1.000000000000000000, 0.000000000000000000 ) ) ;
#15669 = EDGE_CURVE ( 'NONE', #4991, #14019, #2504, .T. ) ;
#15670 = CARTESIAN_POINT ( 'NONE',  ( -40.00000000000000711, 10.00000000000000000, -26.00000000000000000 ) ) ;
#15671 = CLOSED_SHELL ( 'NONE', ( #8351, #5347, #487, #14450, #4439, #10892, #10472, #14457, #1129, #4174, #6764, #37, #13082, #8618, #16657, #16020, #2303, #161, #16607, #8015, #8219, #11082, #8462, #16234, #16023, #15804, #1230, #7703, #9412, #3579, #8772, #6997, #2578, #16743, #15027, #11279, #15491, #13889, #14242, #4084, #16236, #15583, #10544, #14964, #16278, #11340, #7092, #4056, #11778, #1310, #15379, #16660, #15066, #9369, #5270, #4469 ) ) ;
#15672 = EDGE_CURVE ( 'NONE', #3296, #13923, #11620, .T. ) ;
#15673 = DIRECTION ( 'NONE',  ( 0.000000000000000000, 0.000000000000000000, -1.000000000000000000 ) ) ;
#15674 = DIRECTION ( 'NONE',  ( -0.000000000000000000, -1.000000000000000000, -0.000000000000000000 ) ) ;
#15675 = DIRECTION ( 'NONE',  ( 1.000000000000000000, -0.000000000000000000, -0.000000000000000000 ) ) ;
#15676 = CARTESIAN_POINT ( 'NONE',  ( -55.99999999999989342, 549.5810598491749488, -575.3306267969850296 ) ) ;
#15678 = ORIENTED_EDGE ( 'NONE', *, *, #15377, .F. ) ;
#15677 = ORIENTED_EDGE ( 'NONE', *, *, #2895, .F. ) ;
#15679 = EDGE_CURVE ( 'NONE', #8810, #10067, #8879, .T. ) ;
#15680 = CIRCLE ( 'NONE', #7988, 3.300000000000011369 ) ;
#15681 = EDGE_CURVE ( 'NONE', #16499, #14448, #3728, .T. ) ;
#15682 = CARTESIAN_POINT ( 'NONE',  ( 1.250085104875786612E-12, 218.4499468633019603, 287.1312267635915987 ) ) ;
#15683 = ADVANCED_FACE ( 'NONE', ( #6358 ), #1232, .F. ) ;
#15684 = ADVANCED_BREP_SHAPE_REPRESENTATION ( '', ( #2894, #1488 ), #14386 ) ;
#15685 = LINE ( 'NONE', #1267, #12398 ) ;
#15686 = AXIS2_PLACEMENT_3D ( 'NONE', #16385, #678, #7098 ) ;
#15687 = VECTOR ( 'NONE', #7233, 1000.000000000000000 ) ;
#15688 = CARTESIAN_POINT ( 'NONE',  ( -2.220446049250313081E-13, 135.5000000000000000, 3.000000000000000000 ) ) ;
#15689 = DIRECTION ( 'NONE',  ( 0.000000000000000000, -9.899245676326632924E-17, -1.000000000000000000 ) ) ;
#15690 = ORIENTED_EDGE ( 'NONE', *, *, #1021, .T. ) ;
#15691 = CARTESIAN_POINT ( 'NONE',  ( 10.00000000000000000, 425.7506394335853201, -11.00000000000000000 ) ) ;
#15692 = VECTOR ( 'NONE', #6093, 1000.000000000000000 ) ;
#15693 = CARTESIAN_POINT ( 'NONE',  ( 35.99999999999999289, 8.000000000000000000, 21.99999999999999645 ) ) ;
#15695 = ADVANCED_FACE ( 'NONE', ( #11702 ), #12997, .F. ) ;
#15694 = ORIENTED_EDGE ( 'NONE', *, *, #3197, .F. ) ;
#15696 = CYLINDRICAL_SURFACE ( 'NONE', #8063, 18.49999999999998934 ) ;
#15697 = DIRECTION ( 'NONE',  ( 1.000000000000000000, -0.000000000000000000, 0.000000000000000000 ) ) ;
#15698 = CARTESIAN_POINT ( 'NONE',  ( -34.99999999999999289, 8.000000000000000000, 35.00000000000000711 ) ) ;
#15699 = TOROIDAL_SURFACE ( 'NONE', #6640, 4.695405383895982609, 9.000000000000000000 ) ;
#15700 = CARTESIAN_POINT ( 'NONE',  ( 54.99999999999999289, 515.4878487013597805, -359.2230258972048773 ) ) ;
#15701 = VECTOR ( 'NONE', #7953, 1000.000000000000000 ) ;
#15702 = LINE ( 'NONE', #3950, #12970 ) ;
#15703 = VERTEX_POINT ( 'NONE', #16929 ) ;
#15704 = EDGE_CURVE ( 'NONE', #5980, #15749, #10822, .T. ) ;
#15705 = ADVANCED_FACE ( 'NONE', ( #13087 ), #3888, .F. ) ;
#15706 = ADVANCED_FACE ( 'NONE', ( #14462 ), #4066, .F. ) ;
#15707 = DIRECTION ( 'NONE',  ( 0.000000000000000000, 0.9950371902099903743, 0.09950371902098545385 ) ) ;
#15708 = EDGE_CURVE ( 'NONE', #15212, #7469, #16082, .T. ) ;
#15709 = VECTOR ( 'NONE', #2987, 1000.000000000000000 ) ;
#15710 = PLANE ( 'NONE',  #5539 ) ;
#15711 = VECTOR ( 'NONE', #13610, 1000.000000000000227 ) ;
#15712 = VERTEX_POINT ( 'NONE', #14802 ) ;
#15713 = CARTESIAN_POINT ( 'NONE',  ( -3.269999999998768114, 193.4499468632989192, 37.13122676359189711 ) ) ;
#15714 = DIRECTION ( 'NONE',  ( -8.929933532679207200E-16, 0.9950371902099895971, -0.09950371902099479360 ) ) ;
#15715 = LINE ( 'NONE', #3964, #3032 ) ;
#15716 = EDGE_LOOP ( 'NONE', ( #10077, #13935, #10162, #4371, #15956, #6707 ) ) ;
#15717 = CARTESIAN_POINT ( 'NONE',  ( 46.99999999999988631, 473.6663340069157471, -531.5012393965008641 ) ) ;
#15718 = CARTESIAN_POINT ( 'NONE',  ( 0.000000000000000000, 339.4485271457189128, -10.62862937063367852 ) ) ;
#15719 = LINE ( 'NONE', #9115, #16070 ) ;
#15720 = ORIENTED_EDGE ( 'NONE', *, *, #16493, .F. ) ;
#15721 = CIRCLE ( 'NONE', #14069, 2.999999999999995559 ) ;
#15722 = DIRECTION ( 'NONE',  ( -0.000000000000000000, -0.000000000000000000, 1.000000000000000000 ) ) ;
#15723 = ORIENTED_EDGE ( 'NONE', *, *, #15874, .F. ) ;
#15724 = VERTEX_POINT ( 'NONE', #13434 ) ;
#15725 =( GEOMETRIC_REPRESENTATION_CONTEXT ( 3 ) GLOBAL_UNCERTAINTY_ASSIGNED_CONTEXT ( ( #14783 ) ) GLOBAL_UNIT_ASSIGNED_CONTEXT ( ( #16154, #5492, #8252 ) ) REPRESENTATION_CONTEXT ( 'NONE', 'WORKASPACE' ) );
#15726 = LINE ( 'NONE', #3977, #8905 ) ;
#15727 = CIRCLE ( 'NONE', #3130, 13.69540538389601991 ) ;
#15728 = VECTOR ( 'NONE', #12745, 1000.000000000000000 ) ;
#15729 = ORIENTED_EDGE ( 'NONE', *, *, #13198, .T. ) ;
#15730 = ORIENTED_EDGE ( 'NONE', *, *, #5423, .F. ) ;
#15731 = CIRCLE ( 'NONE', #9708, 13.69540538389598794 ) ;
#15732 = ORIENTED_EDGE ( 'NONE', *, *, #69, .F. ) ;
#15733 = LINE ( 'NONE', #3887, #8284 ) ;
#15734 = DIRECTION ( 'NONE',  ( 1.000000000000000000, -0.000000000000000000, 0.000000000000000000 ) ) ;
#15735 =( GEOMETRIC_REPRESENTATION_CONTEXT ( 3 ) GLOBAL_UNCERTAINTY_ASSIGNED_CONTEXT ( ( #9626 ) ) GLOBAL_UNIT_ASSIGNED_CONTEXT ( ( #9724, #13590, #16238 ) ) REPRESENTATION_CONTEXT ( 'NONE', 'WORKASPACE' ) );
#15736 = ORIENTED_EDGE ( 'NONE', *, *, #12571, .F. ) ;
#15737 = DIRECTION ( 'NONE',  ( 0.000000000000000000, 0.000000000000000000, -1.000000000000000000 ) ) ;
#15738 = VECTOR ( 'NONE', #1486, 1000.000000000000000 ) ;
#15739 = EDGE_CURVE ( 'NONE', #9277, #6058, #15477, .T. ) ;
#15740 = FACE_OUTER_BOUND ( 'NONE', #3655, .T. ) ;
#15741 = CIRCLE ( 'NONE', #8353, 30.00000000000002842 ) ;
#15742 = DIRECTION ( 'NONE',  ( 0.000000000000000000, 0.000000000000000000, -1.000000000000000000 ) ) ;
#15743 = ORIENTED_EDGE ( 'NONE', *, *, #7823, .F. ) ;
#15744 = PLANE ( 'NONE',  #11175 ) ;
#15745 = CYLINDRICAL_SURFACE ( 'NONE', #2833, 4.999999999999997335 ) ;
#15746 = ORIENTED_EDGE ( 'NONE', *, *, #8456, .F. ) ;
#15747 = EDGE_CURVE ( 'NONE', #10494, #10121, #6713, .T. ) ;
#15748 = DIRECTION ( 'NONE',  ( 0.000000000000000000, 0.000000000000000000, -1.000000000000000000 ) ) ;
#15749 = VERTEX_POINT ( 'NONE', #9477 ) ;
#15750 = LINE ( 'NONE', #3998, #9771 ) ;
#15751 = AXIS2_PLACEMENT_3D ( 'NONE', #3008, #6056, #16380 ) ;
#15752 = ORIENTED_EDGE ( 'NONE', *, *, #7997, .T. ) ;
#15753 = EDGE_LOOP ( 'NONE', ( #1300, #8343, #12531, #2272 ) ) ;
#15754 = DIRECTION ( 'NONE',  ( 0.000000000000000000, 0.000000000000000000, -1.000000000000000000 ) ) ;
#15755 = EDGE_CURVE ( 'NONE', #14549, #4210, #12049, .T. ) ;
#15756 = AXIS2_PLACEMENT_3D ( 'NONE', #13842, #6004, #13750 ) ;
#15757 = LINE ( 'NONE', #13189, #11011 ) ;
#15758 = ORIENTED_EDGE ( 'NONE', *, *, #1417, .T. ) ;
#15759 = EDGE_CURVE ( 'NONE', #4224, #10447, #5600, .T. ) ;
#15760 = LINE ( 'NONE', #9157, #13511 ) ;
#15761 = PRODUCT_DEFINITION_SHAPE ( 'NONE', 'NONE',  #16971 ) ;
#15762 = CARTESIAN_POINT ( 'NONE',  ( -22.00000000000001776, 6.000000000000000000, 36.00000000000000711 ) ) ;
#15763 = EDGE_CURVE ( 'NONE', #16083, #8414, #8263, .T. ) ;
#15764 = LINE ( 'NONE', #6558, #1898 ) ;
#15765 = CARTESIAN_POINT ( 'NONE',  ( 31.00000000000003553, 0.000000000000000000, -22.99999999999999645 ) ) ;
#15766 = CARTESIAN_POINT ( 'NONE',  ( -26.00000000000002842, 0.000000000000000000, 31.00000000000003908 ) ) ;
#15767 = CIRCLE ( 'NONE', #6419, 13.69540538389601991 ) ;
#15768 = LINE ( 'NONE', #14572, #9720 ) ;
#15769 = FACE_OUTER_BOUND ( 'NONE', #11803, .T. ) ;
#15771 = ORIENTED_EDGE ( 'NONE', *, *, #2548, .T. ) ;
#15770 = EDGE_LOOP ( 'NONE', ( #8432, #7731, #11293, #6689 ) ) ;
#15772 = DIRECTION ( 'NONE',  ( 0.000000000000000000, 0.000000000000000000, 1.000000000000000000 ) ) ;
#15773 = CARTESIAN_POINT ( 'NONE',  ( 0.1475654038900472698, 285.9036875807895512, 37.40882805463662208 ) ) ;
#15774 = EDGE_CURVE ( 'NONE', #5894, #2869, #16032, .T. ) ;
#15775 = CARTESIAN_POINT ( 'NONE',  ( -20.00000000000003197, 3.000000000000000000, 37.00000000000000711 ) ) ;
#15776 = DIRECTION ( 'NONE',  ( -1.000000000000000000, 0.000000000000000000, 0.000000000000000000 ) ) ;
#15777 = ORIENTED_EDGE ( 'NONE', *, *, #8895, .T. ) ;
#15778 = VECTOR ( 'NONE', #749, 1000.000000000000000 ) ;
#15779 = CYLINDRICAL_SURFACE ( 'NONE', #11319, 5.000000000000000888 ) ;
#15780 = EDGE_CURVE ( 'NONE', #452, #9574, #5242, .T. ) ;
#15781 = EDGE_CURVE ( 'NONE', #15647, #4736, #5507, .T. ) ;
#15782 = CARTESIAN_POINT ( 'NONE',  ( -55.99999999999989342, 549.5810598491746077, -518.1154249974242703 ) ) ;
#15783 = EDGE_LOOP ( 'NONE', ( #9877, #10726, #2191, #16541 ) ) ;
#15784 = CARTESIAN_POINT ( 'NONE',  ( 3.000000000000000000, 1.836909530733570325E-16, 3.000000000000000000 ) ) ;
#15785 = DIRECTION ( 'NONE',  ( 0.000000000000000000, 0.000000000000000000, 1.000000000000000000 ) ) ;
#15786 = LINE ( 'NONE', #12351, #14581 ) ;
#15787 = CARTESIAN_POINT ( 'NONE',  ( 55.99999999999989342, 473.6663340069157471, -517.8058340126048051 ) ) ;
#15788 =( NAMED_UNIT ( * ) PLANE_ANGLE_UNIT ( ) SI_UNIT ( $, .RADIAN. ) );
#15789 = DIRECTION ( 'NONE',  ( 0.000000000000000000, 0.000000000000000000, -1.000000000000000000 ) ) ;
#15790 = EDGE_LOOP ( 'NONE', ( #4410, #11140, #14725, #3878 ) ) ;
#15791 = VECTOR ( 'NONE', #13132, 1000.000000000000114 ) ;
#15792 = CARTESIAN_POINT ( 'NONE',  ( -55.99999999999989342, 523.2161522479893847, -604.2478186815853860 ) ) ;
#15793 = VECTOR ( 'NONE', #5580, 1000.000000000000000 ) ;
#15794 =( NAMED_UNIT ( * ) SI_UNIT ( $, .STERADIAN. ) SOLID_ANGLE_UNIT ( ) );
#15795 = EDGE_CURVE ( 'NONE', #2045, #175, #27, .T. ) ;
#15796 = CARTESIAN_POINT ( 'NONE',  ( 55.99999999999989342, 549.5810598491746077, -518.1154249974242703 ) ) ;
#15797 = EDGE_LOOP ( 'NONE', ( #2384, #4078, #3619, #10071 ) ) ;
#15798 = FACE_OUTER_BOUND ( 'NONE', #6347, .T. ) ;
#15799 = UNCERTAINTY_MEASURE_WITH_UNIT (LENGTH_MEASURE( 1.000000000000000082E-05 ), #391, 'distance_accuracy_value', 'NONE');
#15800 = EDGE_CURVE ( 'NONE', #8348, #2142, #9224, .T. ) ;
#15801 = CARTESIAN_POINT ( 'NONE',  ( 46.99999999999988631, 549.5810598491746077, -518.1154249974242703 ) ) ;
#15802 = EDGE_CURVE ( 'NONE', #1311, #2938, #4141, .T. ) ;
#15803 = AXIS2_PLACEMENT_3D ( 'NONE', #2372, #13029, #11732 ) ;
#15804 = ADVANCED_FACE ( 'NONE', ( #3986 ), #14718, .F. ) ;
#15805 = DIRECTION ( 'NONE',  ( 0.000000000000000000, 0.000000000000000000, -1.000000000000000000 ) ) ;
#15806 = ORIENTED_EDGE ( 'NONE', *, *, #9381, .T. ) ;
#15807 = AXIS2_PLACEMENT_3D ( 'NONE', #4291, #10712, #14763 ) ;
#15808 = DIRECTION ( 'NONE',  ( 0.000000000000000000, 1.000000000000000000, 0.000000000000000000 ) ) ;
#15809 = ADVANCED_FACE ( 'NONE', ( #371 ), #2946, .F. ) ;
#15810 = CARTESIAN_POINT ( 'NONE',  ( 2.625000000000000000, -14.59999999999999964, -1.787984326755135766E-15 ) ) ;
#15811 = DIRECTION ( 'NONE',  ( 0.000000000000000000, 0.000000000000000000, -1.000000000000000000 ) ) ;
#15812 = EDGE_LOOP ( 'NONE', ( #13042, #10962, #1551, #6351 ) ) ;
#15813 = PLANE ( 'NONE',  #6130 ) ;
#15814 = ORIENTED_EDGE ( 'NONE', *, *, #2986, .F. ) ;
#15815 = ORIENTED_EDGE ( 'NONE', *, *, #4265, .F. ) ;
#15816 = CARTESIAN_POINT ( 'NONE',  ( -34.99999999999999289, 8.000000000000000000, -35.00000000000000711 ) ) ;
#15817 = ORIENTED_EDGE ( 'NONE', *, *, #14026, .F. ) ;
#15818 = VECTOR ( 'NONE', #15908, 1000.000000000000000 ) ;
#15819 = AXIS2_PLACEMENT_3D ( 'NONE', #16628, #10108, #15344 ) ;
#15820 = ORIENTED_EDGE ( 'NONE', *, *, #3017, .T. ) ;
#15821 = VERTEX_POINT ( 'NONE', #6614 ) ;
#15822 = SHAPE_REPRESENTATION ( 'HG-KN73JK', ( #9434, #672, #4509, #11617, #2572, #14930, #12999, #7502 ), #12184 ) ;
#15823 = LINE ( 'NONE', #9561, #8826 ) ;
#15824 = CARTESIAN_POINT ( 'NONE',  ( -40.00000000000000000, 19.00000000000000000, -26.00000000000000355 ) ) ;
#15825 = ORIENTED_EDGE ( 'NONE', *, *, #9438, .F. ) ;
#15826 = CARTESIAN_POINT ( 'NONE',  ( 46.99999999999988631, 523.2161522479888163, -502.8936384967199729 ) ) ;
#15827 = EDGE_CURVE ( 'NONE', #4810, #4609, #5316, .T. ) ;
#15828 = DIRECTION ( 'NONE',  ( -0.000000000000000000, 1.000000000000000000, -0.000000000000000000 ) ) ;
#15829 = VERTEX_POINT ( 'NONE', #8180 ) ;
#15830 = VECTOR ( 'NONE', #14133, 1000.000000000000000 ) ;
#15831 = DIRECTION ( 'NONE',  ( -6.123031769111888756E-17, 1.000000000000000000, 3.749151804555344967E-33 ) ) ;
#15832 = VERTEX_POINT ( 'NONE', #1653 ) ;
#15833 = LINE ( 'NONE', #9309, #201 ) ;
#15834 = LINE ( 'NONE', #9486, #9408 ) ;
#15835 = ORIENTED_EDGE ( 'NONE', *, *, #16843, .F. ) ;
#15836 = DIRECTION ( 'NONE',  ( 0.000000000000000000, 1.000000000000000000, 1.224646799147353207E-16 ) ) ;
#15837 = VERTEX_POINT ( 'NONE', #12135 ) ;
#15838 = CARTESIAN_POINT ( 'NONE',  ( 0.000000000000000000, 306.0487089519832011, -80.00000000000380851 ) ) ;
#15839 = ORIENTED_EDGE ( 'NONE', *, *, #2921, .F. ) ;
#15840 = CIRCLE ( 'NONE', #4335, 13.69540538389601991 ) ;
#15841 = VERTEX_POINT ( 'NONE', #15824 ) ;
#15842 = CARTESIAN_POINT ( 'NONE',  ( 46.99999999999988631, 559.9933750504617365, -560.4184312811007658 ) ) ;
#15843 = DIRECTION ( 'NONE',  ( 0.000000000000000000, -1.000000000000000000, 0.000000000000000000 ) ) ;
#15844 = DIRECTION ( 'NONE',  ( 0.000000000000000000, 0.000000000000000000, -1.000000000000000000 ) ) ;
#15845 = ORIENTED_EDGE ( 'NONE', *, *, #3018, .T. ) ;
#15846 = LINE ( 'NONE', #11810, #6338 ) ;
#15847 = LINE ( 'NONE', #9410, #13278 ) ;
#15848 = DIRECTION ( 'NONE',  ( 0.000000000000000000, 0.000000000000000000, 1.000000000000000000 ) ) ;
#15849 = LINE ( 'NONE', #405, #3202 ) ;
#15850 = CARTESIAN_POINT ( 'NONE',  ( 46.99999999999988631, 559.9933750504617365, -533.0276205133087615 ) ) ;
#15851 = DIRECTION ( 'NONE',  ( 1.000000000000000000, 0.000000000000000000, -0.000000000000000000 ) ) ;
#15852 = DIRECTION ( 'NONE',  ( 0.000000000000000000, 0.000000000000000000, 1.000000000000000000 ) ) ;
#15854 = ORIENTED_EDGE ( 'NONE', *, *, #13194, .T. ) ;
#15853 = ORIENTED_EDGE ( 'NONE', *, *, #6038, .F. ) ;
#15855 = CARTESIAN_POINT ( 'NONE',  ( 45.00000000000000000, 549.5810598491746077, -531.8108303813202156 ) ) ;
#15856 = CARTESIAN_POINT ( 'NONE',  ( 0.6444877810225767556, 286.1732733541648486, 37.23446286945507921 ) ) ;
#15857 = LINE ( 'NONE', #15775, #582 ) ;
#15858 = CARTESIAN_POINT ( 'NONE',  ( 45.00000000000000000, 473.6663340069158039, -548.2494070140132862 ) ) ;
#15859 = ORIENTED_EDGE ( 'NONE', *, *, #15951, .T. ) ;
#15860 = VECTOR ( 'NONE', #16894, 1000.000000000000000 ) ;
#15861 = DIRECTION ( 'NONE',  ( -0.000000000000000000, -1.000000000000000000, 0.000000000000000000 ) ) ;
#15862 = APPLICATION_CONTEXT ( 'automotive_design' ) ;
#15863 = PLANE ( 'NONE',  #15807 ) ;
#15864 = EDGE_LOOP ( 'NONE', ( #4667, #1123, #12896, #11022 ) ) ;
#15865 = PLANE ( 'NONE',  #14830 ) ;
#15866 = DIRECTION ( 'NONE',  ( 1.000000000000000000, 0.000000000000000000, 0.000000000000000000 ) ) ;
#15867 = CARTESIAN_POINT ( 'NONE',  ( 10.00000000000000000, 364.9870314427736275, -216.3519347178565795 ) ) ;
#15868 = EDGE_CURVE ( 'NONE', #1410, #1496, #8609, .T. ) ;
#15869 = ADVANCED_FACE ( 'NONE', ( #16251 ), #7305, .F. ) ;
#15870 =( LENGTH_UNIT ( ) NAMED_UNIT ( * ) SI_UNIT ( .MILLI., .METRE. ) );
#15871 = DIRECTION ( 'NONE',  ( 0.000000000000000000, 0.000000000000000000, 1.000000000000000000 ) ) ;
#15872 = ORIENTED_EDGE ( 'NONE', *, *, #1439, .F. ) ;
#15873 = DIRECTION ( 'NONE',  ( -1.000000000000000000, 0.000000000000000000, -0.000000000000000000 ) ) ;
#15874 = EDGE_CURVE ( 'NONE', #7289, #15132, #15222, .T. ) ;
#15875 = CARTESIAN_POINT ( 'NONE',  ( -10.00000000000000000, 6.452029775889750974E-16, 5.268482129199949959 ) ) ;
#15876 = AXIS2_PLACEMENT_3D ( 'NONE', #12750, #3646, #7575 ) ;
#15877 = ORIENTED_EDGE ( 'NONE', *, *, #15827, .F. ) ;
#15878 = DIRECTION ( 'NONE',  ( 0.000000000000000000, -0.9271838545667883125, -0.3746065934159096278 ) ) ;
#15879 = DIRECTION ( 'NONE',  ( 1.000000000000000000, 0.000000000000000000, 0.000000000000000000 ) ) ;
#15880 = DIRECTION ( 'NONE',  ( -1.000000000000000000, 0.000000000000000000, 3.854941057726254367E-16 ) ) ;
#15881 = ORIENTED_EDGE ( 'NONE', *, *, #387, .F. ) ;
#15882 = DIRECTION ( 'NONE',  ( -1.000000000000000000, 2.277380563333649802E-16, 0.000000000000000000 ) ) ;
#15883 = CARTESIAN_POINT ( 'NONE',  ( 394.0000000000001137, 339.3157724647196005, -110.6822657433597925 ) ) ;
#15884 = CARTESIAN_POINT ( 'NONE',  ( 56.72999999999999687, 214.4632308570088810, 287.5298983642209123 ) ) ;
#15885 = ORIENTED_EDGE ( 'NONE', *, *, #15291, .F. ) ;
#15886 = ADVANCED_FACE ( 'NONE', ( #8359 ), #462, .T. ) ;
#15887 = VERTEX_POINT ( 'NONE', #1903 ) ;
#15888 = ORIENTED_EDGE ( 'NONE', *, *, #6277, .F. ) ;
#15889 = AXIS2_PLACEMENT_3D ( 'NONE', #16220, #1626, #15962 ) ;
#15890 = PLANE ( 'NONE',  #416 ) ;
#15891 = ORIENTED_EDGE ( 'NONE', *, *, #11917, .T. ) ;
#15892 = ADVANCED_FACE ( 'NONE', ( #14971 ), #11180, .F. ) ;
#15893 = CARTESIAN_POINT ( 'NONE',  ( 27.99999999999992895, -9.810510073395585451, -35.37201075597399580 ) ) ;
#15894 = EDGE_CURVE ( 'NONE', #5917, #9633, #9649, .T. ) ;
#15895 = EDGE_CURVE ( 'NONE', #117, #10651, #4511, .T. ) ;
#15896 = ORIENTED_EDGE ( 'NONE', *, *, #11870, .T. ) ;
#15897 = ORIENTED_EDGE ( 'NONE', *, *, #13301, .T. ) ;
#15898 = FACE_BOUND ( 'NONE', #6988, .T. ) ;
#15899 = CARTESIAN_POINT ( 'NONE',  ( -26.00000000000002842, 0.000000000000000000, 34.00000000000000711 ) ) ;
#15900 = AXIS2_PLACEMENT_3D ( 'NONE', #8552, #4849, #7157 ) ;
#15901 = EDGE_LOOP ( 'NONE', ( #9191, #7499, #2623, #6913 ) ) ;
#15903 = CARTESIAN_POINT ( 'NONE',  ( 0.000000000000000000, 0.000000000000000000, -12.00000000000000178 ) ) ;
#15902 = AXIS2_PLACEMENT_3D ( 'NONE', #13727, #9698, #5733 ) ;
#15904 = DIRECTION ( 'NONE',  ( -0.000000000000000000, -1.000000000000000000, -0.000000000000000000 ) ) ;
#15905 = VERTEX_POINT ( 'NONE', #12555 ) ;
#15906 = DIRECTION ( 'NONE',  ( 1.000000000000000000, 0.000000000000000000, 0.000000000000000000 ) ) ;
#15907 = ORIENTED_EDGE ( 'NONE', *, *, #11384, .F. ) ;
#15908 = DIRECTION ( 'NONE',  ( 1.000000000000000000, 0.000000000000000000, 0.000000000000000000 ) ) ;
#15909 = LINE ( 'NONE', #11976, #10241 ) ;
#15910 = ORIENTED_EDGE ( 'NONE', *, *, #6632, .F. ) ;
#15911 = DIRECTION ( 'NONE',  ( 0.000000000000000000, -0.3746065934159092392, -0.9271838545667885345 ) ) ;
#15912 = VERTEX_POINT ( 'NONE', #14880 ) ;
#15913 = ADVANCED_FACE ( 'NONE', ( #13681 ), #6968, .T. ) ;
#15914 =( LENGTH_UNIT ( ) NAMED_UNIT ( * ) SI_UNIT ( .MILLI., .METRE. ) );
#15915 = EDGE_CURVE ( 'NONE', #3786, #9007, #6687, .T. ) ;
#15916 = LINE ( 'NONE', #6726, #13336 ) ;
#15917 = CIRCLE ( 'NONE', #12901, 10.00000000000000178 ) ;
#15918 = VECTOR ( 'NONE', #2426, 1000.000000000000000 ) ;
#15919 = EDGE_CURVE ( 'NONE', #15132, #1879, #7770, .T. ) ;
#15920 = SHAPE_REPRESENTATION ( 'Part7', ( #1488 ), #3972 ) ;
#15921 = VERTEX_POINT ( 'NONE', #11014 ) ;
#15922 = VERTEX_POINT ( 'NONE', #1832 ) ;
#15923 = CARTESIAN_POINT ( 'NONE',  ( -20.99999999999999645, 19.00000000000000000, 35.00000000000001421 ) ) ;
#15924 = CYLINDRICAL_SURFACE ( 'NONE', #7701, 13.69540538389596485 ) ;
#15925 = CARTESIAN_POINT ( 'NONE',  ( -46.99999999999988631, 559.9933750504617365, -546.7230258972048205 ) ) ;
#15926 = ORIENTED_EDGE ( 'NONE', *, *, #259, .F. ) ;
#15927 = CARTESIAN_POINT ( 'NONE',  ( 31.00000000000006395, 68.00000000000000000, -22.99999999999999289 ) ) ;
#15928 = CARTESIAN_POINT ( 'NONE',  ( 29.68009836720079875, 275.4439001176564830, 0.000000000000000000 ) ) ;
#15929 = AXIS2_PLACEMENT_3D ( 'NONE', #3246, #9778, #9597 ) ;
#15930 = DIRECTION ( 'NONE',  ( 1.000000000000000000, 0.000000000000000000, 0.000000000000000000 ) ) ;
#15931 = DIRECTION ( 'NONE',  ( 0.000000000000000000, 0.000000000000000000, -1.000000000000000000 ) ) ;
#15932 = DIRECTION ( 'NONE',  ( -1.000000000000000000, -0.000000000000000000, -0.000000000000000000 ) ) ;
#15933 = CARTESIAN_POINT ( 'NONE',  ( 31.00000000000003553, 11.00000000000000000, -26.00000000000000355 ) ) ;
#15934 = CARTESIAN_POINT ( 'NONE',  ( 17.99999999999998224, 6.000000000000000000, -35.99999999999999289 ) ) ;
#15935 = DIRECTION ( 'NONE',  ( -0.000000000000000000, 1.000000000000000000, 1.224646799147353207E-16 ) ) ;
#15937 = ORIENTED_EDGE ( 'NONE', *, *, #1524, .T. ) ;
#15936 = ORIENTED_EDGE ( 'NONE', *, *, #3625, .F. ) ;
#15938 = DIRECTION ( 'NONE',  ( -0.000000000000000000, 1.000000000000000000, -2.081668171172169499E-16 ) ) ;
#15939 = VECTOR ( 'NONE', #5623, 1000.000000000000000 ) ;
#15940 = CARTESIAN_POINT ( 'NONE',  ( -3.269999999999630536, 285.9619241655763631, 37.54886512656418063 ) ) ;
#15941 = CARTESIAN_POINT ( 'NONE',  ( -270.0000000000000000, 512.1906115401388888, 0.000000000000000000 ) ) ;
#15942 = DIRECTION ( 'NONE',  ( 0.000000000000000000, -0.7625786632508376739, -0.6468954956981579629 ) ) ;
#15943 = ORIENTED_EDGE ( 'NONE', *, *, #10574, .F. ) ;
#15944 =( GEOMETRIC_REPRESENTATION_CONTEXT ( 3 ) GLOBAL_UNCERTAINTY_ASSIGNED_CONTEXT ( ( #523 ) ) GLOBAL_UNIT_ASSIGNED_CONTEXT ( ( #13317, #9532, #6581 ) ) REPRESENTATION_CONTEXT ( 'NONE', 'WORKASPACE' ) );
#15945 = CLOSED_SHELL ( 'NONE', ( #16013, #13163, #13632, #16406, #10487, #11583, #13196 ) ) ;
#15946 = VECTOR ( 'NONE', #3682, 1000.000000000000000 ) ;
#15947 = LINE ( 'NONE', #4026, #4193 ) ;
#15948 = CARTESIAN_POINT ( 'NONE',  ( -55.99999999999989342, 523.2161522479893847, -576.8570079137933817 ) ) ;
#15949 = EDGE_LOOP ( 'NONE', ( #4827, #10457 ) ) ;
#15950 = DIRECTION ( 'NONE',  ( 1.000000000000000000, 0.000000000000000000, -0.000000000000000000 ) ) ;
#15951 = EDGE_CURVE ( 'NONE', #11860, #15084, #1744, .T. ) ;
#15952 = CARTESIAN_POINT ( 'NONE',  ( 40.00000000000003553, 0.000000000000000000, 20.00000000000000355 ) ) ;
#15953 = CARTESIAN_POINT ( 'NONE',  ( 22.99999999999999289, 0.000000000000000000, 37.00000000000002132 ) ) ;
#15954 = CARTESIAN_POINT ( 'NONE',  ( -3.000000000000000000, 6.000000000000000000, 22.00000000000000000 ) ) ;
#15955 = PLANE ( 'NONE',  #13769 ) ;
#15956 = ORIENTED_EDGE ( 'NONE', *, *, #8483, .T. ) ;
#15957 = TOROIDAL_SURFACE ( 'NONE', #9379, 14.27500000000000036, 0.6999999999999999556 ) ;
#15958 = EDGE_CURVE ( 'NONE', #5994, #5602, #12473, .T. ) ;
#15959 = CARTESIAN_POINT ( 'NONE',  ( 46.99999999999988631, 493.2350855268092573, -571.5705369404290650 ) ) ;
#15960 = VECTOR ( 'NONE', #1877, 1000.000000000000000 ) ;
#15961 = AXIS2_PLACEMENT_3D ( 'NONE', #10000, #3048, #7321 ) ;
#15962 = DIRECTION ( 'NONE',  ( 0.000000000000000000, 0.000000000000000000, 1.000000000000000000 ) ) ;
#15963 = DIRECTION ( 'NONE',  ( -1.000000000000000000, -0.000000000000000000, -0.000000000000000000 ) ) ;
#15964 = VECTOR ( 'NONE', #4389, 1000.000000000000000 ) ;
#15965 = ORIENTED_EDGE ( 'NONE', *, *, #596, .F. ) ;
#15966 = ADVANCED_FACE ( 'NONE', ( #5854 ), #9894, .F. ) ;
#15967 = CARTESIAN_POINT ( 'NONE',  ( -21.00000000000002842, -20.00000000000000000, -32.49999999999999289 ) ) ;
#15968 = PRODUCT_DEFINITION_CONTEXT ( 'detailed design', #11802, 'design' ) ;
#15969 = CARTESIAN_POINT ( 'NONE',  ( -40.00000000000000711, 8.000000000000000000, -19.00000000000000355 ) ) ;
#15970 = DIRECTION ( 'NONE',  ( 0.000000000000000000, 0.000000000000000000, 1.000000000000000000 ) ) ;
#15971 = ORIENTED_EDGE ( 'NONE', *, *, #2267, .T. ) ;
#15972 = DIRECTION ( 'NONE',  ( -1.000000000000000000, -0.000000000000000000, 0.000000000000000000 ) ) ;
#15973 = AXIS2_PLACEMENT_3D ( 'NONE', #4873, #15278, #2210 ) ;
#15974 = CYLINDRICAL_SURFACE ( 'NONE', #15311, 3.300000000000011369 ) ;
#15975 = CARTESIAN_POINT ( 'NONE',  ( 46.99999999999988631, 493.2350855268086320, -503.4847040861888559 ) ) ;
#15976 = ORIENTED_EDGE ( 'NONE', *, *, #16846, .F. ) ;
#15977 = ADVANCED_FACE ( 'NONE', ( #13848 ), #11257, .T. ) ;
#15978 =( LENGTH_UNIT ( ) NAMED_UNIT ( * ) SI_UNIT ( .MILLI., .METRE. ) );
#15979 = ORIENTED_EDGE ( 'NONE', *, *, #14982, .T. ) ;
#15980 = ORIENTED_EDGE ( 'NONE', *, *, #4556, .T. ) ;
#15981 = AXIS2_PLACEMENT_3D ( 'NONE', #5463, #10711, #6669 ) ;
#15982 = CARTESIAN_POINT ( 'NONE',  ( 32.99999999999998579, 8.000000000000000000, 21.99999999999999645 ) ) ;
#15983 = ORIENTED_EDGE ( 'NONE', *, *, #7775, .F. ) ;
#15984 = CARTESIAN_POINT ( 'NONE',  ( 300.0000000000000000, -4.163336342344337027E-14, 10.35193471785655284 ) ) ;
#15985 = CIRCLE ( 'NONE', #3378, 9.000000000000007105 ) ;
#15986 = ORIENTED_EDGE ( 'NONE', *, *, #1544, .T. ) ;
#15987 = ORIENTED_EDGE ( 'NONE', *, *, #4040, .F. ) ;
#15988 = EDGE_CURVE ( 'NONE', #1572, #14413, #16492, .T. ) ;
#15989 = CARTESIAN_POINT ( 'NONE',  ( -18.00000000000001421, 6.000000000000000000, 37.00000000000000711 ) ) ;
#15990 = EDGE_CURVE ( 'NONE', #11329, #4486, #12188, .T. ) ;
#15991 = DIRECTION ( 'NONE',  ( 0.000000000000000000, 0.000000000000000000, 1.000000000000000000 ) ) ;
#15992 = VECTOR ( 'NONE', #14464, 1000.000000000000000 ) ;
#15993 = EDGE_LOOP ( 'NONE', ( #12320, #3293, #8035, #13521 ) ) ;
#15994 = CARTESIAN_POINT ( 'NONE',  ( 1.469576158976824144E-15, 10.00000000000000000, 12.00000000000000178 ) ) ;
#15995 = DIRECTION ( 'NONE',  ( 4.930380657631323236E-32, -0.09950371902099770793, 0.9950371902099891530 ) ) ;
#15996 = EDGE_LOOP ( 'NONE', ( #2760, #2674, #8354, #14353, #11581, #5832, #8421, #3912 ) ) ;
#15997 = EDGE_CURVE ( 'NONE', #16035, #4239, #3685, .T. ) ;
#15998 = AXIS2_PLACEMENT_3D ( 'NONE', #12407, #16519, #647 ) ;
#15999 = CARTESIAN_POINT ( 'NONE',  ( 56.73000000000001108, 217.7170024689955596, 287.2045212030222388 ) ) ;
#16000 = VERTEX_POINT ( 'NONE', #8942 ) ;
#16001 = DIRECTION ( 'NONE',  ( 0.000000000000000000, 0.000000000000000000, -1.000000000000000000 ) ) ;
#16002 = CARTESIAN_POINT ( 'NONE',  ( 0.000000000000000000, 65.20000000000000284, 0.9999999999999976685 ) ) ;
#16003 = VERTEX_POINT ( 'NONE', #12886 ) ;
#16004 = FACE_OUTER_BOUND ( 'NONE', #7542, .T. ) ;
#16005 = EDGE_LOOP ( 'NONE', ( #15198, #4566, #1563, #4787 ) ) ;
#16006 = DIRECTION ( 'NONE',  ( 1.000000000000000000, -1.476083657435421627E-31, -7.888609052210118054E-31 ) ) ;
#16007 = VECTOR ( 'NONE', #15472, 1000.000000000000114 ) ;
#16008 = CARTESIAN_POINT ( 'NONE',  ( 75.00000000000000000, 380.0000000000000000, -7.000000000000006217 ) ) ;
#16009 = EDGE_LOOP ( 'NONE', ( #16751, #6075, #9255, #10238 ) ) ;
#16010 = TOROIDAL_SURFACE ( 'NONE', #13275, 4.695405383895982609, 9.000000000000000000 ) ;
#16011 = ORIENTED_EDGE ( 'NONE', *, *, #10660, .T. ) ;
#16012 = LINE ( 'NONE', #2875, #2807 ) ;
#16013 = ADVANCED_FACE ( 'NONE', ( #1211 ), #7381, .T. ) ;
#16014 = CIRCLE ( 'NONE', #2022, 9.500000000000000000 ) ;
#16015 = DIRECTION ( 'NONE',  ( 0.000000000000000000, 0.000000000000000000, -1.000000000000000000 ) ) ;
#16016 = LINE ( 'NONE', #2786, #16292 ) ;
#16017 = FACE_OUTER_BOUND ( 'NONE', #2453, .T. ) ;
#16018 = AXIS2_PLACEMENT_3D ( 'NONE', #152, #13116, #5276 ) ;
#16019 = DIRECTION ( 'NONE',  ( 0.000000000000000000, 1.000000000000000000, 0.000000000000000000 ) ) ;
#16020 = ADVANCED_FACE ( 'NONE', ( #14262 ), #6179, .F. ) ;
#16021 = AXIS2_PLACEMENT_3D ( 'NONE', #4392, #1558, #10733 ) ;
#16022 = EDGE_CURVE ( 'NONE', #3569, #6167, #2322, .T. ) ;
#16023 = ADVANCED_FACE ( 'NONE', ( #16742 ), #15629, .F. ) ;
#16024 = CARTESIAN_POINT ( 'NONE',  ( -21.00000000000002842, -20.00000000000000000, -34.99999999999999289 ) ) ;
#16025 = EDGE_CURVE ( 'NONE', #4334, #5519, #13932, .T. ) ;
#16026 = LINE ( 'NONE', #14826, #9287 ) ;
#16027 = LINE ( 'NONE', #14663, #13081 ) ;
#16028 = CARTESIAN_POINT ( 'NONE',  ( 25.99999999999996092, 3.000000000000000000, 40.00000000000000711 ) ) ;
#16029 = AXIS2_PLACEMENT_3D ( 'NONE', #1562, #104, #14446 ) ;
#16030 =( GEOMETRIC_REPRESENTATION_CONTEXT ( 3 ) GLOBAL_UNCERTAINTY_ASSIGNED_CONTEXT ( ( #12205 ) ) GLOBAL_UNIT_ASSIGNED_CONTEXT ( ( #3381, #3551, #1914 ) ) REPRESENTATION_CONTEXT ( 'NONE', 'WORKASPACE' ) );
#16031 = DIRECTION ( 'NONE',  ( 0.000000000000000000, 0.000000000000000000, -1.000000000000000000 ) ) ;
#16032 = CIRCLE ( 'NONE', #1770, 14.27500000000000036 ) ;
#16033 = DIRECTION ( 'NONE',  ( 0.000000000000000000, -1.224646799147352714E-16, 1.000000000000000000 ) ) ;
#16035 = VERTEX_POINT ( 'NONE', #11344 ) ;
#16034 = ORIENTED_EDGE ( 'NONE', *, *, #12860, .F. ) ;
#16036 = CARTESIAN_POINT ( 'NONE',  ( 3.000000000000000888, 40.80033764248782546, 9.013878188659974811 ) ) ;
#16037 = AXIS2_PLACEMENT_3D ( 'NONE', #12297, #12216, #4400 ) ;
#16038 = VECTOR ( 'NONE', #7429, 1000.000000000000000 ) ;
#16039 = CARTESIAN_POINT ( 'NONE',  ( 0.09296894633892416326, 285.8190614525348110, 37.43392030153078309 ) ) ;
#16040 = CARTESIAN_POINT ( 'NONE',  ( 415.0210210471910841, 329.6061121441327941, -6.736600000000000144 ) ) ;
#16041 = CARTESIAN_POINT ( 'NONE',  ( 30.99999999999996092, 0.000000000000000000, -30.99999999999999289 ) ) ;
#16042 = ORIENTED_EDGE ( 'NONE', *, *, #14023, .T. ) ;
#16043 = CARTESIAN_POINT ( 'NONE',  ( 10.00000000000000000, 309.2289037985885898, -83.18019484660915452 ) ) ;
#16044 = FACE_OUTER_BOUND ( 'NONE', #7632, .T. ) ;
#16045 = ORIENTED_EDGE ( 'NONE', *, *, #2005, .T. ) ;
#16046 = CARTESIAN_POINT ( 'NONE',  ( 31.00000000000004263, 68.00000000000000000, -25.99999999999999645 ) ) ;
#16047 = AXIS2_PLACEMENT_3D ( 'NONE', #13899, #4545, #5911 ) ;
#16048 = EDGE_CURVE ( 'NONE', #16266, #386, #15383, .T. ) ;
#16049 = PLANE ( 'NONE',  #16638 ) ;
#16050 = CARTESIAN_POINT ( 'NONE',  ( -23.00000000000000000, 68.00000000000000000, -31.00000000000005684 ) ) ;
#16051 = PRODUCT_DEFINITION_SHAPE ( 'NONE', 'NONE',  #16976 ) ;
#16052 = LINE ( 'NONE', #4200, #5266 ) ;
#16053 = LINE ( 'NONE', #15096, #1309 ) ;
#16054 = CARTESIAN_POINT ( 'NONE',  ( 10.00000000000000000, 185.0000000000000568, -1.831360450120427585E-14 ) ) ;
#16055 = ORIENTED_EDGE ( 'NONE', *, *, #9438, .T. ) ;
#16056 = DIRECTION ( 'NONE',  ( 0.000000000000000000, -0.000000000000000000, 1.000000000000000000 ) ) ;
#16057 = FACE_OUTER_BOUND ( 'NONE', #5527, .T. ) ;
#16058 = VECTOR ( 'NONE', #15938, 1000.000000000000000 ) ;
#16059 = EDGE_CURVE ( 'NONE', #7006, #8729, #2155, .T. ) ;
#16060 = FILL_AREA_STYLE ('',( #13577 ) ) ;
#16061 = ORIENTED_EDGE ( 'NONE', *, *, #5181, .F. ) ;
#16062 = FACE_OUTER_BOUND ( 'NONE', #5802, .T. ) ;
#16063 = CARTESIAN_POINT ( 'NONE',  ( 0.000000000000000000, 355.3192028797624857, -44.71049682360899169 ) ) ;
#16064 = FACE_OUTER_BOUND ( 'NONE', #3262, .T. ) ;
#16065 = ORIENTED_EDGE ( 'NONE', *, *, #10938, .F. ) ;
#16066 = CARTESIAN_POINT ( 'NONE',  ( -39.99999999999997868, 3.000000000000000000, -19.99999999999999645 ) ) ;
#16067 = CARTESIAN_POINT ( 'NONE',  ( -45.00000000000000000, 523.2161522479888163, -502.8936384967199729 ) ) ;
#16068 = DIRECTION ( 'NONE',  ( 0.000000000000000000, 0.000000000000000000, -1.000000000000000000 ) ) ;
#16069 = ORIENTED_EDGE ( 'NONE', *, *, #15191, .F. ) ;
#16070 = VECTOR ( 'NONE', #13239, 1000.000000000000000 ) ;
#16071 = CIRCLE ( 'NONE', #16615, 3.299999999999997158 ) ;
#16072 = ORIENTED_EDGE ( 'NONE', *, *, #2049, .T. ) ;
#16073 = ORIENTED_EDGE ( 'NONE', *, *, #10986, .F. ) ;
#16074 = FACE_OUTER_BOUND ( 'NONE', #9119, .T. ) ;
#16075 = VERTEX_POINT ( 'NONE', #11593 ) ;
#16076 = APPLICATION_PROTOCOL_DEFINITION ( 'draft international standard', 'automotive_design', 1998, #13576 ) ;
#16077 = ORIENTED_EDGE ( 'NONE', *, *, #10215, .F. ) ;
#16078 = CIRCLE ( 'NONE', #10875, 12.64814671169700055 ) ;
#16079 = ORIENTED_EDGE ( 'NONE', *, *, #615, .T. ) ;
#16080 = AXIS2_PLACEMENT_3D ( 'NONE', #16648, #4955, #13045 ) ;
#16081 = DIRECTION ( 'NONE',  ( 0.000000000000000000, -1.000000000000000000, 0.000000000000000000 ) ) ;
#16082 = LINE ( 'NONE', #6793, #2034 ) ;
#16083 = VERTEX_POINT ( 'NONE', #14184 ) ;
#16084 = LINE ( 'NONE', #3126, #13548 ) ;
#16085 = LINE ( 'NONE', #10936, #2930 ) ;
#16086 = ORIENTED_EDGE ( 'NONE', *, *, #10984, .T. ) ;
#16087 =( NAMED_UNIT ( * ) SI_UNIT ( $, .STERADIAN. ) SOLID_ANGLE_UNIT ( ) );
#16088 = EDGE_LOOP ( 'NONE', ( #550, #13184, #12585, #8379 ) ) ;
#16089 = DIRECTION ( 'NONE',  ( 7.213771534993946619E-17, 0.09950371902098976984, 0.9950371902099900412 ) ) ;
#16090 = CARTESIAN_POINT ( 'NONE',  ( 0.000000000000000000, 0.000000000000000000, 0.000000000000000000 ) ) ;
#16091 = ORIENTED_EDGE ( 'NONE', *, *, #13721, .F. ) ;
#16092 = VECTOR ( 'NONE', #12685, 1000.000000000000000 ) ;
#16093 = EDGE_CURVE ( 'NONE', #8783, #4809, #16588, .T. ) ;
#16094 = VECTOR ( 'NONE', #9696, 1000.000000000000000 ) ;
#16095 = CARTESIAN_POINT ( 'NONE',  ( 10.00000000000000000, 372.8685141053783241, -143.5198051533979537 ) ) ;
#16096 = ORIENTED_EDGE ( 'NONE', *, *, #13038, .T. ) ;
#16097 = DIRECTION ( 'NONE',  ( 0.000000000000000000, 0.000000000000000000, -1.000000000000000000 ) ) ;
#16098 = ORIENTED_EDGE ( 'NONE', *, *, #14986, .T. ) ;
#16099 =( REPRESENTATION_RELATIONSHIP ('NONE','NONE', #15822, #25 ) REPRESENTATION_RELATIONSHIP_WITH_TRANSFORMATION ( #13060 )SHAPE_REPRESENTATION_RELATIONSHIP( ) );
#16100 = ADVANCED_FACE ( 'NONE', ( #15305 ), #16837, .F. ) ;
#16101 = ORIENTED_EDGE ( 'NONE', *, *, #3118, .F. ) ;
#16102 =( NAMED_UNIT ( * ) SI_UNIT ( $, .STERADIAN. ) SOLID_ANGLE_UNIT ( ) );
#16103 = CARTESIAN_POINT ( 'NONE',  ( 46.99999999999988631, 559.9933750504617365, -542.0276205133087615 ) ) ;
#16104 = CARTESIAN_POINT ( 'NONE',  ( -26.00000000000002842, 3.000000000000000000, -39.99999999999999289 ) ) ;
#16105 = VECTOR ( 'NONE', #10420, 1000.000000000000000 ) ;
#16106 = CIRCLE ( 'NONE', #8971, 13.69540538389599682 ) ;
#16107 = DIRECTION ( 'NONE',  ( 1.000000000000000000, 0.000000000000000000, 0.000000000000000000 ) ) ;
#16108 = DIRECTION ( 'NONE',  ( 0.000000000000000000, -0.9271838545667884235, 0.3746065934159092392 ) ) ;
#16109 = DIRECTION ( 'NONE',  ( -1.631319816340925300E-17, -0.000000000000000000, 1.000000000000000000 ) ) ;
#16110 = DIRECTION ( 'NONE',  ( -0.000000000000000000, 1.000000000000000000, -0.000000000000000000 ) ) ;
#16111 = DIRECTION ( 'NONE',  ( 0.000000000000000000, 0.000000000000000000, 1.000000000000000000 ) ) ;
#16112 = LINE ( 'NONE', #1601, #4989 ) ;
#16113 = EDGE_CURVE ( 'NONE', #9577, #15703, #3617, .T. ) ;
#16114 = DIRECTION ( 'NONE',  ( 0.000000000000000000, 0.000000000000000000, 1.000000000000000000 ) ) ;
#16115 = CARTESIAN_POINT ( 'NONE',  ( -49.99999999999999289, 515.4878487013597805, -486.7230258972047636 ) ) ;
#16117 = ORIENTED_EDGE ( 'NONE', *, *, #3426, .T. ) ;
#16116 = ORIENTED_EDGE ( 'NONE', *, *, #2816, .F. ) ;
#16118 = AXIS2_PLACEMENT_3D ( 'NONE', #6582, #11837, #5899 ) ;
#16119 = CARTESIAN_POINT ( 'NONE',  ( 45.00000000000000000, 523.2161522479888163, -502.8936384967199729 ) ) ;
#16120 = EDGE_CURVE ( 'NONE', #8714, #14722, #7461, .T. ) ;
#16121 = ADVANCED_FACE ( 'NONE', ( #8856 ), #14096, .F. ) ;
#16122 = LINE ( 'NONE', #14836, #11843 ) ;
#16123 = EDGE_CURVE ( 'NONE', #204, #13244, #4482, .T. ) ;
#16124 = DIRECTION ( 'NONE',  ( -1.000000000000000000, 0.000000000000000000, 0.000000000000000000 ) ) ;
#16125 = DIRECTION ( 'NONE',  ( 0.000000000000000000, 0.6468954956981579629, -0.7625786632508376739 ) ) ;
#16126 = ORIENTED_EDGE ( 'NONE', *, *, #9740, .T. ) ;
#16127 = CARTESIAN_POINT ( 'NONE',  ( 25.99999999999996092, 3.000000000000000000, -31.00000000000003197 ) ) ;
#16128 = AXIS2_PLACEMENT_3D ( 'NONE', #16136, #430, #4297 ) ;
#16129 = DIRECTION ( 'NONE',  ( 0.000000000000000000, -0.000000000000000000, -1.000000000000000000 ) ) ;
#16130 = ORIENTED_EDGE ( 'NONE', *, *, #1437, .F. ) ;
#16131 = CARTESIAN_POINT ( 'NONE',  ( -34.99999999999998579, -20.00000000000000000, 23.50000000000000711 ) ) ;
#16132 = CIRCLE ( 'NONE', #9275, 2.999999999999995559 ) ;
#16133 = FACE_OUTER_BOUND ( 'NONE', #12564, .T. ) ;
#16134 = PLANE ( 'NONE',  #875 ) ;
#16135 = DIRECTION ( 'NONE',  ( -0.000000000000000000, -1.000000000000000000, -0.000000000000000000 ) ) ;
#16136 = CARTESIAN_POINT ( 'NONE',  ( 55.99999999999989342, 493.2350855268092573, -585.2659423243250103 ) ) ;
#16137 = CYLINDRICAL_SURFACE ( 'NONE', #3618, 9.500000000000000000 ) ;
#16138 = ORIENTED_EDGE ( 'NONE', *, *, #14460, .F. ) ;
#16139 = DIRECTION ( 'NONE',  ( 0.000000000000000000, 1.000000000000000000, 0.000000000000000000 ) ) ;
#16140 = ADVANCED_FACE ( 'NONE', ( #2403 ), #1120, .F. ) ;
#16141 = EDGE_CURVE ( 'NONE', #8784, #12820, #3788, .T. ) ;
#16142 = DIRECTION ( 'NONE',  ( -6.123031769111888756E-17, 1.000000000000000000, 3.749151804555346336E-33 ) ) ;
#16143 = EDGE_CURVE ( 'NONE', #14628, #6725, #12743, .T. ) ;
#16144 = CARTESIAN_POINT ( 'NONE',  ( -13.11912225705329327, 0.000000000000000000, 0.000000000000000000 ) ) ;
#16145 = ORIENTED_EDGE ( 'NONE', *, *, #12244, .F. ) ;
#16146 = DIRECTION ( 'NONE',  ( -1.000000000000000000, -0.000000000000000000, 0.000000000000000000 ) ) ;
#16147 = PRODUCT_DEFINITION_CONTEXT ( 'detailed design', #15549, 'design' ) ;
#16148 = CARTESIAN_POINT ( 'NONE',  ( 1.530757942277970587E-15, 0.000000000000000000, 24.99999999999999645 ) ) ;
#16149 = ORIENTED_EDGE ( 'NONE', *, *, #6211, .T. ) ;
#16150 = DIRECTION ( 'NONE',  ( 0.000000000000000000, 0.000000000000000000, 1.000000000000000000 ) ) ;
#16151 = DIRECTION ( 'NONE',  ( -1.000000000000000000, 0.000000000000000000, 0.000000000000000000 ) ) ;
#16152 = PLANE ( 'NONE',  #7840 ) ;
#16153 = VERTEX_POINT ( 'NONE', #2579 ) ;
#16154 =( LENGTH_UNIT ( ) NAMED_UNIT ( * ) SI_UNIT ( .MILLI., .METRE. ) );
#16155 = ORIENTED_EDGE ( 'NONE', *, *, #3393, .F. ) ;
#16156 = ORIENTED_EDGE ( 'NONE', *, *, #12980, .F. ) ;
#16157 = DIRECTION ( 'NONE',  ( 1.000000000000000000, 0.000000000000000000, 0.000000000000000000 ) ) ;
#16158 = ORIENTED_EDGE ( 'NONE', *, *, #10271, .T. ) ;
#16159 = DIRECTION ( 'NONE',  ( 1.000000000000000000, 0.000000000000000000, 0.000000000000000000 ) ) ;
#16160 = EDGE_LOOP ( 'NONE', ( #15394, #5807, #14477, #2962 ) ) ;
#16161 = VERTEX_POINT ( 'NONE', #13066 ) ;
#16162 = FACE_BOUND ( 'NONE', #8627, .T. ) ;
#16163 = DIRECTION ( 'NONE',  ( 1.000000000000000000, 0.000000000000000000, 0.000000000000000000 ) ) ;
#16164 = ORIENTED_EDGE ( 'NONE', *, *, #16352, .T. ) ;
#16165 = LINE ( 'NONE', #4144, #16801 ) ;
#16166 = LINE ( 'NONE', #1748, #5110 ) ;
#16167 = ORIENTED_EDGE ( 'NONE', *, *, #1837, .F. ) ;
#16168 = VECTOR ( 'NONE', #5987, 1000.000000000000000 ) ;
#16169 =( NAMED_UNIT ( * ) PLANE_ANGLE_UNIT ( ) SI_UNIT ( $, .RADIAN. ) );
#16170 = EDGE_CURVE ( 'NONE', #7984, #2083, #9361, .T. ) ;
#16171 = ORIENTED_EDGE ( 'NONE', *, *, #758, .F. ) ;
#16172 = LINE ( 'NONE', #1281, #5128 ) ;
#16173 = LINE ( 'NONE', #4418, #13262 ) ;
#16174 = ORIENTED_EDGE ( 'NONE', *, *, #10847, .T. ) ;
#16175 = ORIENTED_EDGE ( 'NONE', *, *, #7758, .T. ) ;
#16176 = DIRECTION ( 'NONE',  ( 0.000000000000000000, 0.000000000000000000, 1.000000000000000000 ) ) ;
#16177 = VERTEX_POINT ( 'NONE', #9279 ) ;
#16178 = ORIENTED_EDGE ( 'NONE', *, *, #9317, .T. ) ;
#16179 = CARTESIAN_POINT ( 'NONE',  ( 45.00000000000000000, 523.2161522479893847, -590.5524132976893270 ) ) ;
#16180 = CIRCLE ( 'NONE', #12893, 2.500000000000002220 ) ;
#16181 = FACE_OUTER_BOUND ( 'NONE', #15202, .T. ) ;
#16182 = DIRECTION ( 'NONE',  ( 0.000000000000000000, 0.000000000000000000, -1.000000000000000000 ) ) ;
#16183 = PRODUCT_RELATED_PRODUCT_CATEGORY ( 'part', '', ( #8239 ) ) ;
#16184 = DIRECTION ( 'NONE',  ( 0.000000000000000000, 0.000000000000000000, -1.000000000000000000 ) ) ;
#16185 = MECHANICAL_DESIGN_GEOMETRIC_PRESENTATION_REPRESENTATION (  '', ( #14543 ), #3840 ) ;
#16186 = PRODUCT_DEFINITION_SHAPE ( 'NONE', 'NONE',  #16979 ) ;
#16187 = CARTESIAN_POINT ( 'NONE',  ( 5.941205806953520074, 15.14120580695428764, 0.000000000000000000 ) ) ;
#16188 = DIRECTION ( 'NONE',  ( 0.000000000000000000, 1.000000000000000000, 0.000000000000000000 ) ) ;
#16189 = CARTESIAN_POINT ( 'NONE',  ( 34.00000000000002842, -20.00000000000000000, 23.00000000000000355 ) ) ;
#16190 = CARTESIAN_POINT ( 'NONE',  ( -440.0000000000000568, 620.7506394335853201, 109.9999999999999858 ) ) ;
#16191 = DIRECTION ( 'NONE',  ( 1.000000000000000000, 0.000000000000000000, 0.000000000000000000 ) ) ;
#16192 = ADVANCED_FACE ( 'NONE', ( #5322 ), #2871, .T. ) ;
#16193 = AXIS2_PLACEMENT_3D ( 'NONE', #11685, #8944, #10317 ) ;
#16194 = CIRCLE ( 'NONE', #12362, 5.000000000000000888 ) ;
#16195 = LINE ( 'NONE', #4434, #8621 ) ;
#16196 = LINE ( 'NONE', #9511, #11236 ) ;
#16198 = EDGE_LOOP ( 'NONE', ( #4467, #447, #7366, #5910 ) ) ;
#16197 = ORIENTED_EDGE ( 'NONE', *, *, #13911, .T. ) ;
#16199 = APPLICATION_CONTEXT ( 'automotive_design' ) ;
#16200 = CARTESIAN_POINT ( 'NONE',  ( 1.512611822017149166, 38.37995103523728346, 9.385845453595075938 ) ) ;
#16201 = PRODUCT_DEFINITION_SHAPE ( 'NONE', 'NONE',  #16487 ) ;
#16202 = PRESENTATION_STYLE_ASSIGNMENT (( #10967 ) ) ;
#16203 = DIRECTION ( 'NONE',  ( 0.000000000000000000, 0.000000000000000000, 1.000000000000000000 ) ) ;
#16204 = DIRECTION ( 'NONE',  ( 0.000000000000000000, -0.000000000000000000, -1.000000000000000000 ) ) ;
#16205 = AXIS2_PLACEMENT_3D ( 'NONE', #7339, #12675, #11465 ) ;
#16206 = ORIENTED_EDGE ( 'NONE', *, *, #6664, .F. ) ;
#16207 = EDGE_CURVE ( 'NONE', #1069, #13742, #1291, .T. ) ;
#16208 = DIRECTION ( 'NONE',  ( 0.000000000000000000, 0.000000000000000000, 1.000000000000000000 ) ) ;
#16209 = EDGE_LOOP ( 'NONE', ( #14558, #4388, #12823, #10096 ) ) ;
#16210 = CARTESIAN_POINT ( 'NONE',  ( -2.216159785453297477E-13, 104.2500000000000142, 0.000000000000000000 ) ) ;
#16211 = EDGE_CURVE ( 'NONE', #12044, #12025, #1553, .T. ) ;
#16212 = CARTESIAN_POINT ( 'NONE',  ( -46.99999999999988631, 493.2350855268092573, -585.2659423243250103 ) ) ;
#16213 = DIRECTION ( 'NONE',  ( -0.000000000000000000, 1.000000000000000000, -0.000000000000000000 ) ) ;
#16214 = EDGE_CURVE ( 'NONE', #16595, #6601, #953, .T. ) ;
#16215 = EDGE_CURVE ( 'NONE', #16177, #11437, #7783, .T. ) ;
#16216 = DIRECTION ( 'NONE',  ( 0.000000000000000000, 0.000000000000000000, 1.000000000000000000 ) ) ;
#16217 =( LENGTH_UNIT ( ) NAMED_UNIT ( * ) SI_UNIT ( .MILLI., .METRE. ) );
#16218 = ORIENTED_EDGE ( 'NONE', *, *, #4061, .F. ) ;
#16219 = CARTESIAN_POINT ( 'NONE',  ( 415.3629108289414944, 306.8565854934392974, -6.736600000000000144 ) ) ;
#16220 = CARTESIAN_POINT ( 'NONE',  ( 0.000000000000000000, 239.4632308570078294, 71.73739990498292229 ) ) ;
#16221 = DIRECTION ( 'NONE',  ( 0.000000000000000000, 0.000000000000000000, -1.000000000000000000 ) ) ;
#16222 = ORIENTED_EDGE ( 'NONE', *, *, #9811, .F. ) ;
#16223 = EDGE_CURVE ( 'NONE', #3191, #11237, #349, .T. ) ;
#16224 = DIRECTION ( 'NONE',  ( 0.000000000000000000, 0.09950371902099770793, -0.9950371902099891530 ) ) ;
#16225 = AXIS2_PLACEMENT_3D ( 'NONE', #6112, #1921, #15238 ) ;
#16226 = DIRECTION ( 'NONE',  ( 0.000000000000000000, 1.000000000000000000, 0.000000000000000000 ) ) ;
#16227 = ORIENTED_EDGE ( 'NONE', *, *, #13931, .F. ) ;
#16228 = LINE ( 'NONE', #5486, #7217 ) ;
#16229 = EDGE_CURVE ( 'NONE', #14494, #9217, #9201, .T. ) ;
#16230 = CARTESIAN_POINT ( 'NONE',  ( 0.000000000000000000, 380.0000000000000000, 0.000000000000000000 ) ) ;
#16231 = CARTESIAN_POINT ( 'NONE',  ( -55.99999999999988631, 334.9272574771864015, -321.9943432880672276 ) ) ;
#16232 = ORIENTED_EDGE ( 'NONE', *, *, #13490, .F. ) ;
#16233 = EDGE_CURVE ( 'NONE', #9234, #3717, #268, .T. ) ;
#16234 = ADVANCED_FACE ( 'NONE', ( #3868 ), #11849, .F. ) ;
#16235 = VECTOR ( 'NONE', #431, 1000.000000000000000 ) ;
#16236 = ADVANCED_FACE ( 'NONE', ( #9456 ), #2926, .T. ) ;
#16237 = VECTOR ( 'NONE', #13651, 1000.000000000000000 ) ;
#16238 =( NAMED_UNIT ( * ) SI_UNIT ( $, .STERADIAN. ) SOLID_ANGLE_UNIT ( ) );
#16239 = COLOUR_RGB ( '', 0.66274510, 0.83137255, 0.94901961) ;
#16240 = ORIENTED_EDGE ( 'NONE', *, *, #9737, .F. ) ;
#16241 = ORIENTED_EDGE ( 'NONE', *, *, #14733, .T. ) ;
#16242 = DIRECTION ( 'NONE',  ( 1.000000000000000000, 0.000000000000000000, 0.000000000000000000 ) ) ;
#16243 = ORIENTED_EDGE ( 'NONE', *, *, #15134, .T. ) ;
#16244 = APPLICATION_PROTOCOL_DEFINITION ( 'draft international standard', 'automotive_design', 1998, #9180 ) ;
#16245 = EDGE_LOOP ( 'NONE', ( #10028, #3817 ) ) ;
#16246 = FACE_OUTER_BOUND ( 'NONE', #9075, .T. ) ;
#16247 = EDGE_LOOP ( 'NONE', ( #1053, #4081 ) ) ;
#16248 = CIRCLE ( 'NONE', #3900, 34.00000000000000000 ) ;
#16249 = CIRCLE ( 'NONE', #12945, 4.695405383896011919 ) ;
#16250 = LINE ( 'NONE', #3455, #15692 ) ;
#16251 = FACE_OUTER_BOUND ( 'NONE', #4167, .T. ) ;
#16252 = ORIENTED_EDGE ( 'NONE', *, *, #14545, .T. ) ;
#16253 = CARTESIAN_POINT ( 'NONE',  ( 0.000000000000000000, 341.0487089519837696, -115.0000000000032969 ) ) ;
#16254 = DIRECTION ( 'NONE',  ( -0.000000000000000000, -1.000000000000000000, 0.000000000000000000 ) ) ;
#16255 = VERTEX_POINT ( 'NONE', #6509 ) ;
#16256 = VECTOR ( 'NONE', #11569, 1000.000000000000000 ) ;
#16257 = ADVANCED_FACE ( 'NONE', ( #11765 ), #411, .T. ) ;
#16258 = CARTESIAN_POINT ( 'NONE',  ( 415.0210210471910841, 329.6061121441327941, -6.736600000000000144 ) ) ;
#16259 = ORIENTED_EDGE ( 'NONE', *, *, #4685, .T. ) ;
#16260 = DIRECTION ( 'NONE',  ( -0.000000000000000000, -1.000000000000000000, 0.000000000000000000 ) ) ;
#16261 = ORIENTED_EDGE ( 'NONE', *, *, #4132, .F. ) ;
#16262 = AXIS2_PLACEMENT_3D ( 'NONE', #4598, #15074, #12582 ) ;
#16263 =( GEOMETRIC_REPRESENTATION_CONTEXT ( 3 ) GLOBAL_UNCERTAINTY_ASSIGNED_CONTEXT ( ( #11391 ) ) GLOBAL_UNIT_ASSIGNED_CONTEXT ( ( #6940, #5665, #1712 ) ) REPRESENTATION_CONTEXT ( 'NONE', 'WORKASPACE' ) );
#16264 = EDGE_LOOP ( 'NONE', ( #13588, #16747, #2615, #5474 ) ) ;
#16265 = CARTESIAN_POINT ( 'NONE',  ( 30.90550859392671157, -60.11391548236650095, 66.87703344121199223 ) ) ;
#16266 = VERTEX_POINT ( 'NONE', #3962 ) ;
#16267 = ORIENTED_EDGE ( 'NONE', *, *, #9008, .T. ) ;
#16268 = DIRECTION ( 'NONE',  ( 1.000000000000000000, 0.000000000000000000, 0.000000000000000000 ) ) ;
#16269 = EDGE_CURVE ( 'NONE', #5545, #8924, #2745, .T. ) ;
#16270 = PLANE ( 'NONE',  #13485 ) ;
#16271 = DIRECTION ( 'NONE',  ( -1.000000000000000000, 1.809417926841269906E-12, 1.809417926841437877E-13 ) ) ;
#16272 = PRESENTATION_LAYER_ASSIGNMENT (  '', '', ( #14342 ) ) ;
#16273 = VECTOR ( 'NONE', #6143, 1000.000000000000000 ) ;
#16274 = CARTESIAN_POINT ( 'NONE',  ( -39.99999999999997868, 3.000000000000000000, -25.99999999999999645 ) ) ;
#16275 = VECTOR ( 'NONE', #4808, 1000.000000000000114 ) ;
#16276 = VECTOR ( 'NONE', #581, 1000.000000000000000 ) ;
#16277 = LINE ( 'NONE', #13867, #15184 ) ;
#16278 = ADVANCED_FACE ( 'NONE', ( #13144 ), #1373, .T. ) ;
#16279 = CARTESIAN_POINT ( 'NONE',  ( 10.00000000000000000, 341.0487089519837696, -96.50000000000331113 ) ) ;
#16280 = CARTESIAN_POINT ( 'NONE',  ( -49.99999999999999289, 515.4878487013597805, -461.7230258972048205 ) ) ;
#16281 = ORIENTED_EDGE ( 'NONE', *, *, #7029, .T. ) ;
#16282 = CARTESIAN_POINT ( 'NONE',  ( 39.75350601975127063, 301.2117639810886089, -6.736600000000000144 ) ) ;
#16283 = PLANE ( 'NONE',  #11867 ) ;
#16284 = VECTOR ( 'NONE', #4727, 1000.000000000000114 ) ;
#16285 = CARTESIAN_POINT ( 'NONE',  ( 17.99999999999998224, 10.00000000000000000, -35.99999999999999289 ) ) ;
#16286 = DIRECTION ( 'NONE',  ( -6.123031769111888756E-17, 1.000000000000000000, 3.749151804555344967E-33 ) ) ;
#16288 = ORIENTED_EDGE ( 'NONE', *, *, #9515, .T. ) ;
#16287 = VERTEX_POINT ( 'NONE', #1464 ) ;
#16289 = PRESENTATION_LAYER_ASSIGNMENT (  '', '', ( #9433 ) ) ;
#16290 = LINE ( 'NONE', #3065, #16601 ) ;
#16291 = VECTOR ( 'NONE', #13286, 1000.000000000000000 ) ;
#16292 = VECTOR ( 'NONE', #6732, 1000.000000000000000 ) ;
#16293 = AXIS2_PLACEMENT_3D ( 'NONE', #7645, #9121, #6350 ) ;
#16294 = DIRECTION ( 'NONE',  ( 1.000000000000000000, 0.000000000000000000, 0.000000000000000000 ) ) ;
#16295 = CARTESIAN_POINT ( 'NONE',  ( 10.00000000000000000, 301.0487089519832011, -80.00000000000387956 ) ) ;
#16296 = VECTOR ( 'NONE', #8427, 1000.000000000000000 ) ;
#16297 = ORIENTED_EDGE ( 'NONE', *, *, #3446, .T. ) ;
#16298 = CIRCLE ( 'NONE', #6400, 10.00000000000000178 ) ;
#16299 =( GEOMETRIC_REPRESENTATION_CONTEXT ( 3 ) GLOBAL_UNCERTAINTY_ASSIGNED_CONTEXT ( ( #16702 ) ) GLOBAL_UNIT_ASSIGNED_CONTEXT ( ( #11505, #14258, #3956 ) ) REPRESENTATION_CONTEXT ( 'NONE', 'WORKASPACE' ) );
#16300 = CARTESIAN_POINT ( 'NONE',  ( 55.99999999999989342, 523.2161522479893847, -585.8570079137933817 ) ) ;
#16301 = ORIENTED_EDGE ( 'NONE', *, *, #10442, .T. ) ;
#16302 = CYLINDRICAL_SURFACE ( 'NONE', #13728, 17.52499999999999858 ) ;
#16303 = AXIS2_PLACEMENT_3D ( 'NONE', #5941, #7127, #8518 ) ;
#16304 = CYLINDRICAL_SURFACE ( 'NONE', #7300, 9.500000000000000000 ) ;
#16305 = DIRECTION ( 'NONE',  ( 0.000000000000000000, 1.000000000000000000, 0.000000000000000000 ) ) ;
#16306 = AXIS2_PLACEMENT_3D ( 'NONE', #7296, #12544, #4718 ) ;
#16307 = PLANE ( 'NONE',  #13314 ) ;
#16308 = CARTESIAN_POINT ( 'NONE',  ( -31.00000000000003553, 8.000000000000000000, -21.00000000000000000 ) ) ;
#16309 = ORIENTED_EDGE ( 'NONE', *, *, #9537, .T. ) ;
#16310 = CYLINDRICAL_SURFACE ( 'NONE', #7521, 13.69540538389601991 ) ;
#16311 = ADVANCED_FACE ( 'NONE', ( #6692 ), #184, .F. ) ;
#16312 = DIRECTION ( 'NONE',  ( 0.6294249519366466039, 0.7770612780724246438, 0.000000000000000000 ) ) ;
#16313 = CIRCLE ( 'NONE', #12199, 4.000164074322309027 ) ;
#16314 = DIRECTION ( 'NONE',  ( 1.000000000000000000, 0.000000000000000000, 0.000000000000000000 ) ) ;
#16315 = EDGE_CURVE ( 'NONE', #3004, #6925, #836, .T. ) ;
#16316 = EDGE_LOOP ( 'NONE', ( #13532, #4016, #4984, #15891 ) ) ;
#16317 = VECTOR ( 'NONE', #13320, 1000.000000000000000 ) ;
#16318 = LINE ( 'NONE', #4550, #5556 ) ;
#16319 = DIRECTION ( 'NONE',  ( 0.000000000000000000, 0.000000000000000000, -1.000000000000000000 ) ) ;
#16320 = ORIENTED_EDGE ( 'NONE', *, *, #10148, .F. ) ;
#16321 = CARTESIAN_POINT ( 'NONE',  ( 1.469576158976824144E-15, 10.00000000000000000, 12.00000000000000178 ) ) ;
#16322 = CARTESIAN_POINT ( 'NONE',  ( 21.00000000000000000, 19.00000000000000000, -35.00000000000000711 ) ) ;
#16323 = CARTESIAN_POINT ( 'NONE',  ( 40.00000000000000711, 11.00000000000000000, -26.00000000000000355 ) ) ;
#16324 = VERTEX_POINT ( 'NONE', #3580 ) ;
#16325 = ORIENTED_EDGE ( 'NONE', *, *, #7546, .F. ) ;
#16326 = ORIENTED_EDGE ( 'NONE', *, *, #287, .F. ) ;
#16327 = CARTESIAN_POINT ( 'NONE',  ( -25.99999999999999645, 0.000000000000000000, 31.00000000000003908 ) ) ;
#16328 = ADVANCED_FACE ( 'NONE', ( #16627 ), #15176, .F. ) ;
#16329 = VECTOR ( 'NONE', #15605, 1000.000000000000000 ) ;
#16330 = CONTEXT_DEPENDENT_SHAPE_REPRESENTATION ( #14014, #1361 ) ;
#16331 = PRODUCT_DEFINITION_SHAPE ( 'NONE', 'NONE',  #16985 ) ;
#16332 = EDGE_CURVE ( 'NONE', #16779, #14988, #8816, .T. ) ;
#16333 = CARTESIAN_POINT ( 'NONE',  ( 10.00000000000000000, 374.2147300931088694, -220.2054496871573974 ) ) ;
#16334 = ADVANCED_FACE ( 'NONE', ( #9857 ), #1006, .F. ) ;
#16335 = EDGE_CURVE ( 'NONE', #3442, #6368, #12514, .T. ) ;
#16336 = ORIENTED_EDGE ( 'NONE', *, *, #8829, .F. ) ;
#16337 = EDGE_CURVE ( 'NONE', #1233, #6598, #8242, .T. ) ;
#16338 = CARTESIAN_POINT ( 'NONE',  ( 0.000000000000000000, 376.0487089519837127, -155.0000000000033253 ) ) ;
#16339 = DIRECTION ( 'NONE',  ( 0.000000000000000000, -0.000000000000000000, -1.000000000000000000 ) ) ;
#16340 = ORIENTED_EDGE ( 'NONE', *, *, #15681, .T. ) ;
#16341 = AXIS2_PLACEMENT_3D ( 'NONE', #14896, #1763, #475 ) ;
#16342 = CARTESIAN_POINT ( 'NONE',  ( 5.569974746830579804, 1.808800229719333629E-15, 14.76997474683060041 ) ) ;
#16343 = DIRECTION ( 'NONE',  ( 0.000000000000000000, 0.000000000000000000, -1.000000000000000000 ) ) ;
#16344 = VERTEX_POINT ( 'NONE', #2282 ) ;
#16345 = ORIENTED_EDGE ( 'NONE', *, *, #2341, .T. ) ;
#16346 = EDGE_LOOP ( 'NONE', ( #4152, #16428, #15033, #12909 ) ) ;
#16347 = ORIENTED_EDGE ( 'NONE', *, *, #10667, .T. ) ;
#16348 = SHAPE_REPRESENTATION_RELATIONSHIP ( 'NONE' , 'NONE' ,  #584, #1973 ) ;
#16349 = VECTOR ( 'NONE', #16810, 1000.000000000000000 ) ;
#16350 = VECTOR ( 'NONE', #13564, 1000.000000000000000 ) ;
#16351 = ORIENTED_EDGE ( 'NONE', *, *, #12461, .F. ) ;
#16352 = EDGE_CURVE ( 'NONE', #8801, #8170, #14072, .T. ) ;
#16353 = ORIENTED_EDGE ( 'NONE', *, *, #14865, .F. ) ;
#16354 = LINE ( 'NONE', #9833, #7450 ) ;
#16355 = EDGE_CURVE ( 'NONE', #11568, #4345, #7260, .T. ) ;
#16356 = DIRECTION ( 'NONE',  ( 0.000000000000000000, 0.000000000000000000, 1.000000000000000000 ) ) ;
#16357 = DIRECTION ( 'NONE',  ( 0.000000000000000000, 0.000000000000000000, -1.000000000000000000 ) ) ;
#16358 = FACE_OUTER_BOUND ( 'NONE', #4067, .T. ) ;
#16359 = DIRECTION ( 'NONE',  ( 0.000000000000000000, -0.3853514969300962378, -0.9227698650333863162 ) ) ;
#16360 = VECTOR ( 'NONE', #12518, 1000.000000000000000 ) ;
#16361 = DIRECTION ( 'NONE',  ( 6.123031769111888756E-17, 0.000000000000000000, 1.000000000000000000 ) ) ;
#16362 = AXIS2_PLACEMENT_3D ( 'NONE', #8739, #2031, #10027 ) ;
#16363 = DIRECTION ( 'NONE',  ( -1.000000000000000000, 0.000000000000000000, 4.956352788505159323E-16 ) ) ;
#16364 = ORIENTED_EDGE ( 'NONE', *, *, #10988, .F. ) ;
#16365 = LINE ( 'NONE', #4597, #2657 ) ;
#16366 = PLANE ( 'NONE',  #8026 ) ;
#16367 = CARTESIAN_POINT ( 'NONE',  ( -3.270000000000000462, 220.1329686874181562, 287.5298983642209123 ) ) ;
#16368 = DIRECTION ( 'NONE',  ( -0.000000000000000000, -1.000000000000000000, -0.000000000000000000 ) ) ;
#16370 = EDGE_LOOP ( 'NONE', ( #5780, #13695, #11080, #15965 ) ) ;
#16369 = EDGE_LOOP ( 'NONE', ( #3925, #7431, #10109, #11913 ) ) ;
#16371 = CARTESIAN_POINT ( 'NONE',  ( 0.1972064085032624869, 38.00000000000002132, 9.500000000000005329 ) ) ;
#16372 = CONTEXT_DEPENDENT_SHAPE_REPRESENTATION ( #6987, #8387 ) ;
#16373 = ORIENTED_EDGE ( 'NONE', *, *, #3050, .T. ) ;
#16374 = VECTOR ( 'NONE', #4432, 1000.000000000000000 ) ;
#16375 = CARTESIAN_POINT ( 'NONE',  ( -22.99999999999999645, 0.000000000000000000, -36.99999999999999289 ) ) ;
#16376 = CIRCLE ( 'NONE', #13874, 13.69540538389601636 ) ;
#16377 = PLANE ( 'NONE',  #8804 ) ;
#16378 = LINE ( 'NONE', #5897, #8605 ) ;
#16379 = ORIENTED_EDGE ( 'NONE', *, *, #16332, .T. ) ;
#16380 = DIRECTION ( 'NONE',  ( 6.123031769111888756E-17, 0.000000000000000000, 1.000000000000000000 ) ) ;
#16381 = CARTESIAN_POINT ( 'NONE',  ( 0.7366000000000088033, 192.7170024689980323, 37.20452120302199006 ) ) ;
#16382 = ORIENTED_EDGE ( 'NONE', *, *, #11937, .F. ) ;
#16383 = CARTESIAN_POINT ( 'NONE',  ( -2.693790225569811625, 61.33495048777871261, 9.110418847747206783 ) ) ;
#16384 = CARTESIAN_POINT ( 'NONE',  ( 0.3656342590597776443, 192.8227990814932298, 37.32816098065109145 ) ) ;
#16385 = CARTESIAN_POINT ( 'NONE',  ( 394.0000000000001137, 339.1725919290084335, -111.4188657433597456 ) ) ;
#16386 = VECTOR ( 'NONE', #5135, 1000.000000000000000 ) ;
#16387 = CARTESIAN_POINT ( 'NONE',  ( 46.99999999999988631, 549.5810598491749488, -589.0260321808809749 ) ) ;
#16388 = LINE ( 'NONE', #593, #14762 ) ;
#16389 = EDGE_LOOP ( 'NONE', ( #5952, #4939 ) ) ;
#16390 = DIRECTION ( 'NONE',  ( 7.213771534993946619E-17, 0.09950371902098976984, 0.9950371902099900412 ) ) ;
#16391 = DIRECTION ( 'NONE',  ( 0.000000000000000000, 1.000000000000000000, 0.000000000000000000 ) ) ;
#16392 = EDGE_LOOP ( 'NONE', ( #8982, #8587, #39, #9986 ) ) ;
#16393 =( NAMED_UNIT ( * ) PLANE_ANGLE_UNIT ( ) SI_UNIT ( $, .RADIAN. ) );
#16394 = VECTOR ( 'NONE', #12602, 1000.000000000000000 ) ;
#16395 = ORIENTED_EDGE ( 'NONE', *, *, #8529, .T. ) ;
#16396 = FACE_OUTER_BOUND ( 'NONE', #1758, .T. ) ;
#16397 = EDGE_CURVE ( 'NONE', #3029, #4278, #6147, .T. ) ;
#16398 = FACE_OUTER_BOUND ( 'NONE', #13167, .T. ) ;
#16399 = ORIENTED_EDGE ( 'NONE', *, *, #1854, .F. ) ;
#16400 = DIRECTION ( 'NONE',  ( 0.000000000000000000, 0.000000000000000000, -1.000000000000000000 ) ) ;
#16401 = LINE ( 'NONE', #4472, #9576 ) ;
#16402 = DIRECTION ( 'NONE',  ( -1.000000000000000000, -0.000000000000000000, -0.000000000000000000 ) ) ;
#16403 = ORIENTED_EDGE ( 'NONE', *, *, #15990, .T. ) ;
#16404 = VERTEX_POINT ( 'NONE', #759 ) ;
#16405 = EDGE_LOOP ( 'NONE', ( #6416, #2084, #2248, #1846 ) ) ;
#16406 = ADVANCED_FACE ( 'NONE', ( #6220 ), #4308, .T. ) ;
#16407 = CARTESIAN_POINT ( 'NONE',  ( 25.99999999999999645, 0.000000000000000000, 40.00000000000002132 ) ) ;
#16408 = VECTOR ( 'NONE', #4838, 1000.000000000000000 ) ;
#16409 = APPLICATION_PROTOCOL_DEFINITION ( 'draft international standard', 'automotive_design', 1998, #15862 ) ;
#16410 = CARTESIAN_POINT ( 'NONE',  ( 25.99999999999999645, 11.00000000000000000, 40.00000000000000711 ) ) ;
#16411 = ORIENTED_EDGE ( 'NONE', *, *, #15524, .T. ) ;
#16412 = CARTESIAN_POINT ( 'NONE',  ( 25.99999999999998224, 10.00000000000000000, -31.00000000000003197 ) ) ;
#16413 = DIRECTION ( 'NONE',  ( -2.556703065963790763E-16, 1.000000000000000000, -0.000000000000000000 ) ) ;
#16414 = EDGE_CURVE ( 'NONE', #3142, #14915, #7518, .T. ) ;
#16415 = ORIENTED_EDGE ( 'NONE', *, *, #6459, .F. ) ;
#16416 = DIRECTION ( 'NONE',  ( 0.000000000000000000, 0.000000000000000000, -1.000000000000000000 ) ) ;
#16417 = VECTOR ( 'NONE', #403, 1000.000000000000000 ) ;
#16418 = EDGE_CURVE ( 'NONE', #2365, #2521, #13493, .T. ) ;
#16419 = CARTESIAN_POINT ( 'NONE',  ( 449.9999999999998295, 104.2500000000000142, 0.000000000000000000 ) ) ;
#16420 = EDGE_LOOP ( 'NONE', ( #9563, #15615 ) ) ;
#16421 = CARTESIAN_POINT ( 'NONE',  ( 54.99999999999999289, 515.4878487013597805, -461.7230258972048205 ) ) ;
#16422 = EDGE_CURVE ( 'NONE', #1391, #9705, #1717, .T. ) ;
#16423 = EDGE_LOOP ( 'NONE', ( #724, #9406, #15980, #5902 ) ) ;
#16424 = ORIENTED_EDGE ( 'NONE', *, *, #10168, .T. ) ;
#16425 = EDGE_CURVE ( 'NONE', #1983, #1641, #16313, .T. ) ;
#16426 = EDGE_CURVE ( 'NONE', #16499, #11502, #12681, .T. ) ;
#16427 = ORIENTED_EDGE ( 'NONE', *, *, #15997, .F. ) ;
#16428 = ORIENTED_EDGE ( 'NONE', *, *, #9636, .F. ) ;
#16429 = ORIENTED_EDGE ( 'NONE', *, *, #5116, .F. ) ;
#16430 = CARTESIAN_POINT ( 'NONE',  ( -2.979937318121947509, 40.60126023706489917, 9.020623939867236984 ) ) ;
#16431 = CARTESIAN_POINT ( 'NONE',  ( -22.00000000000001776, 10.00000000000000000, 32.00000000000000711 ) ) ;
#16432 = CYLINDRICAL_SURFACE ( 'NONE', #9715, 10.00000000000000178 ) ;
#16433 = CIRCLE ( 'NONE', #9037, 36.50000000000000000 ) ;
#16434 = EDGE_CURVE ( 'NONE', #5558, #5021, #2113, .T. ) ;
#16435 = DIRECTION ( 'NONE',  ( 0.000000000000000000, 0.000000000000000000, 1.000000000000000000 ) ) ;
#16436 = CARTESIAN_POINT ( 'NONE',  ( 3.000000000000000000, 1.836909530733565148E-16, 12.50000000000000000 ) ) ;
#16437 = CARTESIAN_POINT ( 'NONE',  ( -40.00000000000000711, 8.000000000000000000, -19.00000000000000355 ) ) ;
#16438 = CARTESIAN_POINT ( 'NONE',  ( -2.467345170749142724, 191.0231794615330045, 37.60878752180606455 ) ) ;
#16439 = DIRECTION ( 'NONE',  ( -1.000000000000000000, 0.000000000000000000, 0.000000000000000000 ) ) ;
#16440 = EDGE_CURVE ( 'NONE', #9725, #15129, #12427, .T. ) ;
#16441 = ORIENTED_EDGE ( 'NONE', *, *, #3543, .T. ) ;
#16442 = DIRECTION ( 'NONE',  ( -1.000000000000000000, -0.000000000000000000, -0.000000000000000000 ) ) ;
#16443 = LINE ( 'NONE', #4521, #2819 ) ;
#16444 = ADVANCED_FACE ( 'NONE', ( #8569 ), #9066, .F. ) ;
#16445 = EDGE_CURVE ( 'NONE', #21, #13474, #5887, .T. ) ;
#16446 = DIRECTION ( 'NONE',  ( 0.000000000000000000, 0.000000000000000000, -1.000000000000000000 ) ) ;
#16447 = CARTESIAN_POINT ( 'NONE',  ( -1.776356839400249676E-15, -13.94999999999999929, -1.708382284810557762E-15 ) ) ;
#16449 = ORIENTED_EDGE ( 'NONE', *, *, #3415, .F. ) ;
#16448 = EDGE_LOOP ( 'NONE', ( #8296, #5732, #16599, #7990 ) ) ;
#16450 = DIRECTION ( 'NONE',  ( 0.000000000000000000, 0.000000000000000000, 1.000000000000000000 ) ) ;
#16451 = CIRCLE ( 'NONE', #7386, 4.999999999999997335 ) ;
#16452 = EDGE_LOOP ( 'NONE', ( #105, #1278, #468, #5786 ) ) ;
#16453 = LINE ( 'NONE', #15082, #1678 ) ;
#16454 = CARTESIAN_POINT ( 'NONE',  ( -1.776356839400249676E-15, 0.000000000000000000, 0.000000000000000000 ) ) ;
#16455 = ORIENTED_EDGE ( 'NONE', *, *, #5272, .F. ) ;
#16456 = CARTESIAN_POINT ( 'NONE',  ( -5.000000000000000888, 2.751018388195357790E-15, -22.46376988133006236 ) ) ;
#16457 = AXIS2_PLACEMENT_3D ( 'NONE', #4180, #15935, #16033 ) ;
#16458 = DIRECTION ( 'NONE',  ( 0.000000000000000000, -1.000000000000000000, 0.000000000000000000 ) ) ;
#16459 = ORIENTED_EDGE ( 'NONE', *, *, #15672, .F. ) ;
#16460 = DIRECTION ( 'NONE',  ( -1.000000000000000000, 0.000000000000000000, 0.000000000000000000 ) ) ;
#16461 = CIRCLE ( 'NONE', #4655, 3.299999999999997158 ) ;
#16462 = LINE ( 'NONE', #15267, #16360 ) ;
#16463 = CARTESIAN_POINT ( 'NONE',  ( 31.81980515339464333, 8.000000000000000000, -28.51980515339463906 ) ) ;
#16464 = CYLINDRICAL_SURFACE ( 'NONE', #426, 20.75209553982837463 ) ;
#16465 = PLANE ( 'NONE',  #3512 ) ;
#16466 = VERTEX_POINT ( 'NONE', #14398 ) ;
#16467 = DIRECTION ( 'NONE',  ( 0.000000000000000000, 1.000000000000000000, 0.000000000000000000 ) ) ;
#16468 = VECTOR ( 'NONE', #12148, 1000.000000000000000 ) ;
#16469 = CARTESIAN_POINT ( 'NONE',  ( 5.162501635565829972, 12.32407335584850117, 0.000000000000000000 ) ) ;
#16470 = VERTEX_POINT ( 'NONE', #5185 ) ;
#16471 = SHAPE_REPRESENTATION ( 'Part3', ( #1488 ), #13292 ) ;
#16472 = ORIENTED_EDGE ( 'NONE', *, *, #686, .T. ) ;
#16473 = FACE_OUTER_BOUND ( 'NONE', #2961, .T. ) ;
#16474 = DIRECTION ( 'NONE',  ( -1.000000000000000000, -0.000000000000000000, -0.000000000000000000 ) ) ;
#16475 = ORIENTED_EDGE ( 'NONE', *, *, #14259, .F. ) ;
#16476 = CARTESIAN_POINT ( 'NONE',  ( -31.00000000000001776, 10.00000000000000000, 31.00000000000000000 ) ) ;
#16477 = CARTESIAN_POINT ( 'NONE',  ( 0.000000000000000000, 339.1725919290087745, -9.945665743359786148 ) ) ;
#16478 = CARTESIAN_POINT ( 'NONE',  ( -31.81980515339462912, 11.00000000000000000, -35.11980515339465114 ) ) ;
#16479 = VERTEX_POINT ( 'NONE', #2533 ) ;
#16480 = EDGE_CURVE ( 'NONE', #7289, #1572, #11106, .T. ) ;
#16481 = DIRECTION ( 'NONE',  ( -0.000000000000000000, -1.000000000000000000, -0.000000000000000000 ) ) ;
#16482 = DIRECTION ( 'NONE',  ( 0.000000000000000000, 0.9848077530122062440, 0.1736481776669404620 ) ) ;
#16483 = ORIENTED_EDGE ( 'NONE', *, *, #5798, .F. ) ;
#16484 = ORIENTED_EDGE ( 'NONE', *, *, #13301, .F. ) ;
#16485 = DIRECTION ( 'NONE',  ( 0.000000000000000000, 0.000000000000000000, -1.000000000000000000 ) ) ;
#16486 = APPLICATION_PROTOCOL_DEFINITION ( 'draft international standard', 'automotive_design', 1998, #5331 ) ;
#16487 = PRODUCT_DEFINITION ( 'UNKNOWN', '', #1504, #8654 ) ;
#16488 = CARTESIAN_POINT ( 'NONE',  ( 2.979937318121946177, 60.39873976293512214, 9.020623939867238761 ) ) ;
#16489 = AXIS2_PLACEMENT_3D ( 'NONE', #6990, #14990, #396 ) ;
#16490 = ORIENTED_EDGE ( 'NONE', *, *, #3216, .F. ) ;
#16491 = CARTESIAN_POINT ( 'NONE',  ( 49.99999999999999289, 515.4878487013597805, -546.7230258972048205 ) ) ;
#16492 = LINE ( 'NONE', #3369, #8903 ) ;
#16493 = EDGE_CURVE ( 'NONE', #7690, #7474, #5848, .T. ) ;
#16494 = ORIENTED_EDGE ( 'NONE', *, *, #12028, .T. ) ;
#16495 = DIRECTION ( 'NONE',  ( 0.000000000000000000, 1.000000000000000000, -1.224646799147353207E-16 ) ) ;
#16496 = CLOSED_SHELL ( 'NONE', ( #920, #7261, #15695, #898, #10869, #5829, #1023, #16328, #1109, #11880, #9195, #8678, #14676, #3425 ) ) ;
#16497 = STYLED_ITEM ( 'NONE', ( #7162 ), #14078 ) ;
#16498 = CARTESIAN_POINT ( 'NONE',  ( 46.99999999999988631, 493.2350855268086320, -521.8755148539809170 ) ) ;
#16499 = VERTEX_POINT ( 'NONE', #5022 ) ;
#16500 = CARTESIAN_POINT ( 'NONE',  ( -31.00000000000002842, 68.00000000000000000, -25.99999999999999645 ) ) ;
#16501 = VERTEX_POINT ( 'NONE', #14303 ) ;
#16502 = ORIENTED_EDGE ( 'NONE', *, *, #2268, .F. ) ;
#16503 = AXIS2_PLACEMENT_3D ( 'NONE', #9648, #4407, #8261 ) ;
#16504 = VERTEX_POINT ( 'NONE', #1166 ) ;
#16505 = AXIS2_PLACEMENT_3D ( 'NONE', #12160, #7071, #6901 ) ;
#16506 = ADVANCED_FACE ( 'NONE', ( #6472 ), #11729, .T. ) ;
#16507 = CIRCLE ( 'NONE', #7447, 9.000000000000007105 ) ;
#16508 = VECTOR ( 'NONE', #12168, 1000.000000000000000 ) ;
#16509 = COLOUR_RGB ( '', 0.40784314, 0.44705882, 0.49803922) ;
#16510 = ORIENTED_EDGE ( 'NONE', *, *, #13636, .T. ) ;
#16511 = ORIENTED_EDGE ( 'NONE', *, *, #8704, .T. ) ;
#16512 = CARTESIAN_POINT ( 'NONE',  ( -45.00000000000000000, 549.5810598491749488, -561.6352214130889706 ) ) ;
#16513 = CARTESIAN_POINT ( 'NONE',  ( -20.99999999999999645, 19.00000000000000000, 35.00000000000001421 ) ) ;
#16514 = CARTESIAN_POINT ( 'NONE',  ( -45.00000000000000000, 515.4878487013597805, -606.7230258972047068 ) ) ;
#16515 = VECTOR ( 'NONE', #7713, 1000.000000000000000 ) ;
#16516 = EDGE_CURVE ( 'NONE', #13244, #204, #15215, .T. ) ;
#16517 = CARTESIAN_POINT ( 'NONE',  ( 22.99999999999998224, 10.00000000000000000, -31.00000000000003197 ) ) ;
#16518 = DIRECTION ( 'NONE',  ( -0.000000000000000000, -0.000000000000000000, 1.000000000000000000 ) ) ;
#16519 = DIRECTION ( 'NONE',  ( -0.000000000000000000, -1.000000000000000000, 0.000000000000000000 ) ) ;
#16520 = PLANE ( 'NONE',  #3278 ) ;
#16521 = DIRECTION ( 'NONE',  ( 1.000000000000000000, -0.000000000000000000, 0.000000000000000000 ) ) ;
#16522 = VECTOR ( 'NONE', #5745, 1000.000000000000000 ) ;
#16523 = EDGE_LOOP ( 'NONE', ( #13079, #2333, #2542, #3688 ) ) ;
#16524 = CARTESIAN_POINT ( 'NONE',  ( -31.00000000000003553, 19.00000000000000000, -21.00000000000000000 ) ) ;
#16525 = FACE_OUTER_BOUND ( 'NONE', #630, .T. ) ;
#16526 = DIRECTION ( 'NONE',  ( 1.000000000000000000, 0.000000000000000000, -0.000000000000000000 ) ) ;
#16528 = ORIENTED_EDGE ( 'NONE', *, *, #7089, .T. ) ;
#16527 = VERTEX_POINT ( 'NONE', #1253 ) ;
#16529 = AXIS2_PLACEMENT_3D ( 'NONE', #15361, #7616, #14323 ) ;
#16530 = FACE_OUTER_BOUND ( 'NONE', #6867, .T. ) ;
#16531 = EDGE_CURVE ( 'NONE', #11631, #7648, #4008, .T. ) ;
#16532 = ORIENTED_EDGE ( 'NONE', *, *, #1086, .F. ) ;
#16533 = CARTESIAN_POINT ( 'NONE',  ( 25.99999999999997868, 0.000000000000000000, -39.99999999999999289 ) ) ;
#16534 = AXIS2_PLACEMENT_3D ( 'NONE', #8450, #14000, #6247 ) ;
#16535 = VECTOR ( 'NONE', #11220, 1000.000000000000000 ) ;
#16536 = CARTESIAN_POINT ( 'NONE',  ( 30.99999999999999645, 3.000000000000000000, 26.00000000000000355 ) ) ;
#16537 = EDGE_CURVE ( 'NONE', #49, #9826, #16875, .T. ) ;
#16538 = DIRECTION ( 'NONE',  ( 1.000000000000000000, -0.000000000000000000, 0.000000000000000000 ) ) ;
#16539 = EDGE_CURVE ( 'NONE', #9815, #9087, #16953, .T. ) ;
#16541 = ORIENTED_EDGE ( 'NONE', *, *, #12459, .T. ) ;
#16540 = EDGE_CURVE ( 'NONE', #11116, #16479, #14630, .T. ) ;
#16542 = EDGE_CURVE ( 'NONE', #8468, #14313, #1081, .T. ) ;
#16543 = DIRECTION ( 'NONE',  ( 1.000000000000000000, 0.000000000000000000, 0.000000000000000000 ) ) ;
#16544 = VECTOR ( 'NONE', #9564, 1000.000000000000000 ) ;
#16545 = CARTESIAN_POINT ( 'NONE',  ( -36.99999999999997868, 3.000000000000000000, -22.99999999999999645 ) ) ;
#16546 = VERTEX_POINT ( 'NONE', #6297 ) ;
#16547 = FACE_OUTER_BOUND ( 'NONE', #15056, .T. ) ;
#16548 = CARTESIAN_POINT ( 'NONE',  ( -3.000000000000000000, -1.836909530733565148E-16, 22.00000000000000000 ) ) ;
#16549 = FACE_OUTER_BOUND ( 'NONE', #10590, .T. ) ;
#16550 = AXIS2_PLACEMENT_3D ( 'NONE', #14146, #10284, #2444 ) ;
#16551 = PLANE ( 'NONE',  #13285 ) ;
#16552 = VECTOR ( 'NONE', #10253, 1000.000000000000000 ) ;
#16553 = CARTESIAN_POINT ( 'NONE',  ( 25.99999999999999645, 68.00000000000000000, 31.00000000000004619 ) ) ;
#16554 = EDGE_LOOP ( 'NONE', ( #7919, #7773, #6630, #8652 ) ) ;
#16555 = CARTESIAN_POINT ( 'NONE',  ( 45.00000000000000000, 493.2350855268092573, -585.2659423243250103 ) ) ;
#16556 = CARTESIAN_POINT ( 'NONE',  ( 55.99999999999989342, 473.6663340069158039, -561.9448123979092315 ) ) ;
#16557 = ORIENTED_EDGE ( 'NONE', *, *, #8793, .F. ) ;
#16558 = PLANE ( 'NONE',  #15973 ) ;
#16559 = ADVANCED_FACE ( 'NONE', ( #7938 ), #5112, .F. ) ;
#16560 = ORIENTED_EDGE ( 'NONE', *, *, #7608, .T. ) ;
#16561 = VECTOR ( 'NONE', #9132, 1000.000000000000000 ) ;
#16562 = EDGE_CURVE ( 'NONE', #1196, #4760, #1476, .T. ) ;
#16563 = VECTOR ( 'NONE', #1574, 1000.000000000000000 ) ;
#16564 = DIRECTION ( 'NONE',  ( 0.000000000000000000, 0.000000000000000000, -1.000000000000000000 ) ) ;
#16565 = DIRECTION ( 'NONE',  ( 0.000000000000000000, 0.000000000000000000, -1.000000000000000000 ) ) ;
#16566 = VERTEX_POINT ( 'NONE', #15425 ) ;
#16567 = CARTESIAN_POINT ( 'NONE',  ( -30.99999999999999645, 0.000000000000000000, -30.99999999999999289 ) ) ;
#16568 = AXIS2_PLACEMENT_3D ( 'NONE', #8999, #2451, #11651 ) ;
#16569 = CYLINDRICAL_SURFACE ( 'NONE', #11746, 13.69540538389601991 ) ;
#16570 = LINE ( 'NONE', #9880, #14438 ) ;
#16571 = ORIENTED_EDGE ( 'NONE', *, *, #1960, .T. ) ;
#16572 = VECTOR ( 'NONE', #11324, 1000.000000000000000 ) ;
#16573 = PRODUCT_DEFINITION_SHAPE ( 'NONE', 'NONE',  #12202 ) ;
#16574 =( NAMED_UNIT ( * ) PLANE_ANGLE_UNIT ( ) SI_UNIT ( $, .RADIAN. ) );
#16575 = DIRECTION ( 'NONE',  ( 3.854941057726251409E-16, 0.000000000000000000, 1.000000000000000000 ) ) ;
#16576 = CARTESIAN_POINT ( 'NONE',  ( -1.281199806755509263, 288.9467639778929424, 37.61247111518800068 ) ) ;
#16577 = VERTEX_POINT ( 'NONE', #10189 ) ;
#16578 = VERTEX_POINT ( 'NONE', #7763 ) ;
#16579 = DIRECTION ( 'NONE',  ( 1.000000000000000000, 0.000000000000000000, 0.000000000000000000 ) ) ;
#16580 =( GEOMETRIC_REPRESENTATION_CONTEXT ( 3 ) GLOBAL_UNCERTAINTY_ASSIGNED_CONTEXT ( ( #5668 ) ) GLOBAL_UNIT_ASSIGNED_CONTEXT ( ( #4828, #4909, #7229 ) ) REPRESENTATION_CONTEXT ( 'NONE', 'WORKASPACE' ) );
#16581 = VECTOR ( 'NONE', #96, 1000.000000000000000 ) ;
#16582 = PRODUCT_CONTEXT ( 'NONE', #4131, 'mechanical' ) ;
#16583 =( NAMED_UNIT ( * ) PLANE_ANGLE_UNIT ( ) SI_UNIT ( $, .RADIAN. ) );
#16584 = AXIS2_PLACEMENT_3D ( 'NONE', #5592, #9291, #7985 ) ;
#16585 = DIRECTION ( 'NONE',  ( 0.000000000000000000, 0.000000000000000000, -1.000000000000000000 ) ) ;
#16586 = ORIENTED_EDGE ( 'NONE', *, *, #16059, .F. ) ;
#16587 = LINE ( 'NONE', #16412, #4970 ) ;
#16588 = LINE ( 'NONE', #4817, #13567 ) ;
#16589 = PRODUCT_DEFINITION_FORMATION_WITH_SPECIFIED_SOURCE ( 'ANY', '', #13025, .NOT_KNOWN. ) ;
#16590 = VERTEX_POINT ( 'NONE', #3829 ) ;
#16591 = DIRECTION ( 'NONE',  ( -1.000000000000000000, -3.474153781073083121E-15, -3.474153781073041508E-16 ) ) ;
#16592 = DIRECTION ( 'NONE',  ( -0.000000000000000000, -1.000000000000000000, -0.000000000000000000 ) ) ;
#16593 = ORIENTED_EDGE ( 'NONE', *, *, #4584, .T. ) ;
#16594 = CARTESIAN_POINT ( 'NONE',  ( 56.73000000000000398, 189.4632308570087105, 37.52989836422094072 ) ) ;
#16595 = VERTEX_POINT ( 'NONE', #3916 ) ;
#16596 = EDGE_LOOP ( 'NONE', ( #15503, #6499 ) ) ;
#16597 = ORIENTED_EDGE ( 'NONE', *, *, #14551, .F. ) ;
#16598 = ORIENTED_EDGE ( 'NONE', *, *, #10271, .F. ) ;
#16599 = ORIENTED_EDGE ( 'NONE', *, *, #521, .T. ) ;
#16600 = DIRECTION ( 'NONE',  ( 0.000000000000000000, -1.000000000000000000, 0.000000000000000000 ) ) ;
#16601 = VECTOR ( 'NONE', #1785, 1000.000000000000000 ) ;
#16602 = DIRECTION ( 'NONE',  ( -1.000000000000000000, 0.000000000000000000, -1.734723475976807094E-15 ) ) ;
#16603 = DIRECTION ( 'NONE',  ( 0.000000000000000000, 0.000000000000000000, -1.000000000000000000 ) ) ;
#16604 = DIRECTION ( 'NONE',  ( -1.000000000000000000, -0.000000000000000000, -0.000000000000000000 ) ) ;
#16605 = LINE ( 'NONE', #12828, #7750 ) ;
#16606 = DIRECTION ( 'NONE',  ( 3.854941057726249930E-16, 0.000000000000000000, 1.000000000000000000 ) ) ;
#16607 = ADVANCED_FACE ( 'NONE', ( #9248 ), #8909, .F. ) ;
#16608 = DIRECTION ( 'NONE',  ( -0.000000000000000000, -1.000000000000000000, -0.000000000000000000 ) ) ;
#16609 = EDGE_CURVE ( 'NONE', #11059, #1839, #14089, .T. ) ;
#16610 = FACE_OUTER_BOUND ( 'NONE', #3596, .T. ) ;
#16611 = ORIENTED_EDGE ( 'NONE', *, *, #10988, .T. ) ;
#16612 = DIRECTION ( 'NONE',  ( -0.000000000000000000, -1.000000000000000000, -0.000000000000000000 ) ) ;
#16613 = CARTESIAN_POINT ( 'NONE',  ( 25.99999999999996092, 0.000000000000000000, -31.00000000000003197 ) ) ;
#16614 = AXIS2_PLACEMENT_3D ( 'NONE', #4980, #16914, #4049 ) ;
#16615 = AXIS2_PLACEMENT_3D ( 'NONE', #13447, #1669, #16176 ) ;
#16616 = PLANE ( 'NONE',  #10414 ) ;
#16618 = ORIENTED_EDGE ( 'NONE', *, *, #7517, .T. ) ;
#16617 = VERTEX_POINT ( 'NONE', #6902 ) ;
#16619 = ADVANCED_FACE ( 'NONE', ( #12163, #400 ), #8202, .F. ) ;
#16620 = DIRECTION ( 'NONE',  ( -1.631319816340925608E-17, 8.952264470854156086E-17, 1.000000000000000000 ) ) ;
#16621 = ORIENTED_EDGE ( 'NONE', *, *, #16434, .T. ) ;
#16622 = CARTESIAN_POINT ( 'NONE',  ( 10.00000000000000000, 214.9999999999953104, -486.7326477857724853 ) ) ;
#16623 = CYLINDRICAL_SURFACE ( 'NONE', #8251, 7.500000000000007105 ) ;
#16624 = PLANE ( 'NONE',  #6658 ) ;
#16625 = AXIS2_PLACEMENT_3D ( 'NONE', #11243, #1971, #15206 ) ;
#16626 = ORIENTED_EDGE ( 'NONE', *, *, #11717, .T. ) ;
#16627 = FACE_OUTER_BOUND ( 'NONE', #4946, .T. ) ;
#16628 = CARTESIAN_POINT ( 'NONE',  ( 45.00000000000000000, 473.6663340069157471, -531.5012393965008641 ) ) ;
#16630 = EDGE_CURVE ( 'NONE', #5706, #7594, #5016, .T. ) ;
#16629 = ORIENTED_EDGE ( 'NONE', *, *, #15167, .T. ) ;
#16631 = CARTESIAN_POINT ( 'NONE',  ( -45.00000000000000000, 473.6663340069157471, -545.1966447803968094 ) ) ;
#16632 = CARTESIAN_POINT ( 'NONE',  ( -1.745738565991610924, 190.2524942469967755, 37.61874632382036054 ) ) ;
#16633 = CARTESIAN_POINT ( 'NONE',  ( 449.9999999999998295, 135.5000000000000000, 3.000000000000000000 ) ) ;
#16634 = DIRECTION ( 'NONE',  ( -1.000000000000000000, 0.000000000000000000, -0.000000000000000000 ) ) ;
#16635 = DIRECTION ( 'NONE',  ( -0.000000000000000000, -1.000000000000000000, -0.000000000000000000 ) ) ;
#16636 = ORIENTED_EDGE ( 'NONE', *, *, #3935, .F. ) ;
#16637 = EDGE_CURVE ( 'NONE', #10595, #2493, #660, .T. ) ;
#16638 = AXIS2_PLACEMENT_3D ( 'NONE', #4197, #5468, #14767 ) ;
#16639 = EDGE_CURVE ( 'NONE', #7051, #7178, #15847, .T. ) ;
#16640 = CARTESIAN_POINT ( 'NONE',  ( -440.0000000000000568, 620.7506394335853201, 109.9999999999999858 ) ) ;
#16641 = VECTOR ( 'NONE', #760, 1000.000000000000000 ) ;
#16642 = EDGE_CURVE ( 'NONE', #14988, #594, #488, .T. ) ;
#16643 = DIRECTION ( 'NONE',  ( 0.000000000000000000, 0.000000000000000000, -1.000000000000000000 ) ) ;
#16644 = DIRECTION ( 'NONE',  ( -1.000000000000000000, 0.000000000000000000, -0.000000000000000000 ) ) ;
#16645 = ORIENTED_EDGE ( 'NONE', *, *, #890, .F. ) ;
#16646 = DIRECTION ( 'NONE',  ( 0.000000000000000000, 0.000000000000000000, 1.000000000000000000 ) ) ;
#16647 = AXIS2_PLACEMENT_3D ( 'NONE', #10507, #1319, #13355 ) ;
#16648 = CARTESIAN_POINT ( 'NONE',  ( -40.00000000000000711, 10.00000000000000000, 26.00000000000000000 ) ) ;
#16649 = VERTEX_POINT ( 'NONE', #16187 ) ;
#16650 = DIRECTION ( 'NONE',  ( 0.000000000000000000, 0.000000000000000000, -1.000000000000000000 ) ) ;
#16651 = LINE ( 'NONE', #5048, #16677 ) ;
#16652 = FACE_OUTER_BOUND ( 'NONE', #11108, .T. ) ;
#16653 = ORIENTED_EDGE ( 'NONE', *, *, #1515, .T. ) ;
#16654 = LINE ( 'NONE', #10055, #14754 ) ;
#16655 = FACE_OUTER_BOUND ( 'NONE', #6193, .T. ) ;
#16656 = VERTEX_POINT ( 'NONE', #4089 ) ;
#16657 = ADVANCED_FACE ( 'NONE', ( #14743 ), #2882, .F. ) ;
#16658 = ADVANCED_FACE ( 'NONE', ( #1677 ), #10874, .F. ) ;
#16659 = CARTESIAN_POINT ( 'NONE',  ( 55.99999999999989342, 473.6663340069158039, -561.9448123979092315 ) ) ;
#16660 = ADVANCED_FACE ( 'NONE', ( #4428 ), #9675, .F. ) ;
#16661 = CONTEXT_DEPENDENT_SHAPE_REPRESENTATION ( #4586, #12353 ) ;
#16662 = PRESENTATION_LAYER_ASSIGNMENT (  '', '', ( #7055 ) ) ;
#16663 = CARTESIAN_POINT ( 'NONE',  ( -3.000000000000000000, -1.836909530733565148E-16, 3.000000000000000000 ) ) ;
#16664 = ORIENTED_EDGE ( 'NONE', *, *, #15292, .F. ) ;
#16665 = CARTESIAN_POINT ( 'NONE',  ( 0.000000000000000000, 240.7889724647196488, -104.2090657433598011 ) ) ;
#16666 = CARTESIAN_POINT ( 'NONE',  ( -31.81980515339462912, 8.000000000000000000, -31.81980515339465043 ) ) ;
#16667 = VERTEX_POINT ( 'NONE', #15928 ) ;
#16668 = DIRECTION ( 'NONE',  ( -0.000000000000000000, -1.000000000000000000, -0.000000000000000000 ) ) ;
#16669 = CARTESIAN_POINT ( 'NONE',  ( 10.00000000000000000, 381.0487089519832011, -80.00000000000332534 ) ) ;
#16670 = EDGE_LOOP ( 'NONE', ( #10230, #110, #8976, #13785 ) ) ;
#16671 = CARTESIAN_POINT ( 'NONE',  ( 10.00000000000000000, 306.0487089519837127, -150.0000000000038369 ) ) ;
#16672 = VERTEX_POINT ( 'NONE', #1597 ) ;
#16673 = ORIENTED_EDGE ( 'NONE', *, *, #9077, .F. ) ;
#16674 = ORIENTED_EDGE ( 'NONE', *, *, #12150, .T. ) ;
#16675 = EDGE_LOOP ( 'NONE', ( #13834, #16364, #5231, #15979 ) ) ;
#16676 = ORIENTED_EDGE ( 'NONE', *, *, #9940, .F. ) ;
#16677 = VECTOR ( 'NONE', #8840, 1000.000000000000000 ) ;
#16678 = CARTESIAN_POINT ( 'NONE',  ( -30.99999999999999289, 0.000000000000000000, 31.00000000000000000 ) ) ;
#16679 = DIRECTION ( 'NONE',  ( -0.000000000000000000, -1.000000000000000000, -0.000000000000000000 ) ) ;
#16680 = FACE_OUTER_BOUND ( 'NONE', #10214, .T. ) ;
#16681 = CARTESIAN_POINT ( 'NONE',  ( -150.0000000000000284, 620.7506394335853201, -11.00000000000000000 ) ) ;
#16682 = DIRECTION ( 'NONE',  ( 1.000000000000000000, 0.000000000000000000, 0.000000000000000000 ) ) ;
#16683 = EDGE_CURVE ( 'NONE', #10598, #11589, #12074, .T. ) ;
#16684 = LINE ( 'NONE', #8722, #15375 ) ;
#16685 = CARTESIAN_POINT ( 'NONE',  ( -25.99999999999999645, 0.000000000000000000, 40.00000000000002132 ) ) ;
#16686 = ORIENTED_EDGE ( 'NONE', *, *, #7826, .F. ) ;
#16687 = DIRECTION ( 'NONE',  ( 0.000000000000000000, 1.000000000000000000, 0.000000000000000000 ) ) ;
#16688 = DIRECTION ( 'NONE',  ( 1.000000000000000000, -0.000000000000000000, -0.000000000000000000 ) ) ;
#16689 = ORIENTED_EDGE ( 'NONE', *, *, #7486, .F. ) ;
#16690 = EDGE_CURVE ( 'NONE', #10651, #117, #4746, .T. ) ;
#16691 = TOROIDAL_SURFACE ( 'NONE', #8482, 4.695405383895982609, 9.000000000000000000 ) ;
#16692 = CYLINDRICAL_SURFACE ( 'NONE', #13183, 30.00000000000002842 ) ;
#16694 = ORIENTED_EDGE ( 'NONE', *, *, #15195, .F. ) ;
#16693 = ORIENTED_EDGE ( 'NONE', *, *, #6201, .T. ) ;
#16695 = DIRECTION ( 'NONE',  ( 0.000000000000000000, 1.000000000000000000, 1.321694076934710402E-16 ) ) ;
#16696 = AXIS2_PLACEMENT_3D ( 'NONE', #8356, #4814, #9891 ) ;
#16697 = DIRECTION ( 'NONE',  ( 1.000000000000000000, 0.000000000000000000, -0.000000000000000000 ) ) ;
#16698 = PRODUCT_RELATED_PRODUCT_CATEGORY ( 'part', '', ( #13025 ) ) ;
#16699 = DIRECTION ( 'NONE',  ( -0.000000000000000000, 0.000000000000000000, -1.000000000000000000 ) ) ;
#16700 = CARTESIAN_POINT ( 'NONE',  ( 0.000000000000000000, 380.0000000000000000, 0.000000000000000000 ) ) ;
#16701 = VERTEX_POINT ( 'NONE', #1514 ) ;
#16702 = UNCERTAINTY_MEASURE_WITH_UNIT (LENGTH_MEASURE( 1.000000000000000082E-05 ), #11505, 'distance_accuracy_value', 'NONE');
#16703 = CARTESIAN_POINT ( 'NONE',  ( -54.99999999999999289, 515.4878487013597805, -546.7230258972048205 ) ) ;
#16704 = EDGE_CURVE ( 'NONE', #5519, #11776, #5366, .T. ) ;
#16705 = CARTESIAN_POINT ( 'NONE',  ( 30.99999999999997513, 0.000000000000000000, 30.99999999999999645 ) ) ;
#16706 = ORIENTED_EDGE ( 'NONE', *, *, #15499, .F. ) ;
#16707 = CARTESIAN_POINT ( 'NONE',  ( 23.00000000000000711, 68.00000000000000000, -31.00000000000002487 ) ) ;
#16708 = FACE_BOUND ( 'NONE', #15623, .T. ) ;
#16709 = CYLINDRICAL_SURFACE ( 'NONE', #3356, 13.69540538389601991 ) ;
#16710 = VECTOR ( 'NONE', #1457, 1000.000000000000000 ) ;
#16711 = DIRECTION ( 'NONE',  ( -1.000000000000000000, -0.000000000000000000, -1.631319816340925608E-17 ) ) ;
#16712 = DIRECTION ( 'NONE',  ( -0.000000000000000000, 1.000000000000000000, -0.000000000000000000 ) ) ;
#16713 = ORIENTED_EDGE ( 'NONE', *, *, #15499, .T. ) ;
#16714 = DIRECTION ( 'NONE',  ( 0.000000000000000000, 0.000000000000000000, -1.000000000000000000 ) ) ;
#16715 = DIRECTION ( 'NONE',  ( 0.000000000000000000, 1.000000000000000000, 0.000000000000000000 ) ) ;
#16716 = EDGE_CURVE ( 'NONE', #7341, #6882, #4351, .T. ) ;
#16717 = CARTESIAN_POINT ( 'NONE',  ( -9.000000000000001776, 0.000000000000000000, 22.50000000000003908 ) ) ;
#16718 = AXIS2_PLACEMENT_3D ( 'NONE', #6565, #15602, #3836 ) ;
#16719 = ORIENTED_EDGE ( 'NONE', *, *, #11656, .T. ) ;
#16720 = VECTOR ( 'NONE', #2727, 1000.000000000000000 ) ;
#16721 = DIRECTION ( 'NONE',  ( 1.000000000000000000, -0.000000000000000000, 0.000000000000000000 ) ) ;
#16722 = EDGE_CURVE ( 'NONE', #7813, #1375, #10240, .T. ) ;
#16723 = CARTESIAN_POINT ( 'NONE',  ( 31.99999999999998579, 10.00000000000000000, 25.99999999999999645 ) ) ;
#16724 = ORIENTED_EDGE ( 'NONE', *, *, #15591, .F. ) ;
#16725 = LINE ( 'NONE', #12868, #1920 ) ;
#16726 = DIRECTION ( 'NONE',  ( -1.000000000000000000, 0.000000000000000000, 6.123233995736766036E-17 ) ) ;
#16727 = DIRECTION ( 'NONE',  ( 0.000000000000000000, 0.000000000000000000, -1.000000000000000000 ) ) ;
#16728 = ORIENTED_EDGE ( 'NONE', *, *, #4886, .T. ) ;
#16729 =( NAMED_UNIT ( * ) PLANE_ANGLE_UNIT ( ) SI_UNIT ( $, .RADIAN. ) );
#16730 = CARTESIAN_POINT ( 'NONE',  ( -39.99999999999997868, 3.000000000000000000, 26.00000000000000355 ) ) ;
#16731 = PLANE ( 'NONE',  #9701 ) ;
#16732 = EDGE_LOOP ( 'NONE', ( #9694, #11790, #4627, #10464 ) ) ;
#16733 = CARTESIAN_POINT ( 'NONE',  ( 31.00000000000000000, 19.00000000000000000, 30.99999999999999289 ) ) ;
#16734 = CIRCLE ( 'NONE', #8792, 8.999999999999952038 ) ;
#16735 = CONTEXT_DEPENDENT_SHAPE_REPRESENTATION ( #11703, #7937 ) ;
#16736 = APPLICATION_CONTEXT ( 'automotive_design' ) ;
#16737 = EDGE_CURVE ( 'NONE', #2600, #7389, #2556, .T. ) ;
#16738 = ADVANCED_FACE ( 'NONE', ( #3152 ), #14565, .F. ) ;
#16739 = ORIENTED_EDGE ( 'NONE', *, *, #14583, .F. ) ;
#16740 = DIRECTION ( 'NONE',  ( 5.782411586589399054E-16, 0.000000000000000000, -1.000000000000000000 ) ) ;
#16741 = ADVANCED_FACE ( 'NONE', ( #10695 ), #737, .T. ) ;
#16742 = FACE_OUTER_BOUND ( 'NONE', #603, .T. ) ;
#16743 = ADVANCED_FACE ( 'NONE', ( #4660 ), #8798, .T. ) ;
#16744 = CIRCLE ( 'NONE', #314, 9.000000000000007105 ) ;
#16745 = EDGE_CURVE ( 'NONE', #7960, #3043, #16277, .T. ) ;
#16746 = LINE ( 'NONE', #1374, #9896 ) ;
#16747 = ORIENTED_EDGE ( 'NONE', *, *, #3012, .F. ) ;
#16748 = DIRECTION ( 'NONE',  ( 0.000000000000000000, 0.000000000000000000, -1.000000000000000000 ) ) ;
#16749 = ADVANCED_FACE ( 'NONE', ( #1853 ), #3229, .F. ) ;
#16750 = CARTESIAN_POINT ( 'NONE',  ( -22.99999999999999645, 68.00000000000000000, -36.99999999999999289 ) ) ;
#16751 = ORIENTED_EDGE ( 'NONE', *, *, #10062, .F. ) ;
#16752 = FACE_OUTER_BOUND ( 'NONE', #3965, .T. ) ;
#16753 = ORIENTED_EDGE ( 'NONE', *, *, #11684, .F. ) ;
#16754 = EDGE_LOOP ( 'NONE', ( #16864, #4395, #4646, #12916 ) ) ;
#16755 = CARTESIAN_POINT ( 'NONE',  ( 0.000000000000000000, 341.0487089519837696, -133.5000000000032969 ) ) ;
#16756 = ORIENTED_EDGE ( 'NONE', *, *, #3706, .T. ) ;
#16757 = DIRECTION ( 'NONE',  ( 1.335138895993184054E-16, 0.000000000000000000, 1.000000000000000000 ) ) ;
#16758 = ORIENTED_EDGE ( 'NONE', *, *, #13395, .F. ) ;
#16759 = ORIENTED_EDGE ( 'NONE', *, *, #782, .T. ) ;
#16760 = DIRECTION ( 'NONE',  ( 0.000000000000000000, 0.000000000000000000, -1.000000000000000000 ) ) ;
#16761 = CARTESIAN_POINT ( 'NONE',  ( 10.00000000000000000, 376.0487089519831443, -75.00000000000331113 ) ) ;
#16762 = DIRECTION ( 'NONE',  ( -0.000000000000000000, -0.000000000000000000, -1.000000000000000000 ) ) ;
#16763 = CARTESIAN_POINT ( 'NONE',  ( 18.99999999999998224, 10.00000000000000000, -39.99999999999999289 ) ) ;
#16764 = ADVANCED_FACE ( 'NONE', ( #8461 ), #4516, .F. ) ;
#16765 = CARTESIAN_POINT ( 'NONE',  ( -46.99999999999988631, 473.6663340069157471, -526.8058340126048051 ) ) ;
#16766 = AXIS2_PLACEMENT_3D ( 'NONE', #4329, #16081, #12303 ) ;
#16767 = LINE ( 'NONE', #5002, #3549 ) ;
#16768 = DIRECTION ( 'NONE',  ( 0.000000000000000000, 0.000000000000000000, 1.000000000000000000 ) ) ;
#16769 = EDGE_LOOP ( 'NONE', ( #12392, #757, #13349, #3200, #4972 ) ) ;
#16770 = CARTESIAN_POINT ( 'NONE',  ( -31.00000000000007105, 10.00000000000000000, 23.00000000000000000 ) ) ;
#16771 = PLANE ( 'NONE',  #7211 ) ;
#16772 = EDGE_LOOP ( 'NONE', ( #14655, #2355, #12609, #14707, #2324 ) ) ;
#16773 = VECTOR ( 'NONE', #5473, 1000.000000000000000 ) ;
#16774 = AXIS2_PLACEMENT_3D ( 'NONE', #4092, #1427, #5635 ) ;
#16775 = CARTESIAN_POINT ( 'NONE',  ( 394.0000000000001137, 339.4485271457185718, -110.7359021160857537 ) ) ;
#16777 = ORIENTED_EDGE ( 'NONE', *, *, #7604, .F. ) ;
#16776 = ORIENTED_EDGE ( 'NONE', *, *, #3803, .F. ) ;
#16778 = DIRECTION ( 'NONE',  ( 0.000000000000000000, 0.000000000000000000, 1.000000000000000000 ) ) ;
#16779 = VERTEX_POINT ( 'NONE', #4593 ) ;
#16780 = EDGE_CURVE ( 'NONE', #8520, #1501, #7073, .T. ) ;
#16781 = CIRCLE ( 'NONE', #8002, 6.473199999999998511 ) ;
#16782 =( NAMED_UNIT ( * ) SI_UNIT ( $, .STERADIAN. ) SOLID_ANGLE_UNIT ( ) );
#16783 = PLANE ( 'NONE',  #8813 ) ;
#16784 = PLANE ( 'NONE',  #13264 ) ;
#16785 = ORIENTED_EDGE ( 'NONE', *, *, #67, .F. ) ;
#16786 = VECTOR ( 'NONE', #7941, 1000.000000000000000 ) ;
#16787 = AXIS2_PLACEMENT_3D ( 'NONE', #13063, #2739, #1286 ) ;
#16788 = CARTESIAN_POINT ( 'NONE',  ( -26.00000000000002132, 10.00000000000000000, 40.00000000000000711 ) ) ;
#16789 = EDGE_LOOP ( 'NONE', ( #15313, #10116, #12947, #2866, #4863, #14235, #8108, #13687 ) ) ;
#16790 = DIRECTION ( 'NONE',  ( -1.000000000000000000, 0.000000000000000000, -0.000000000000000000 ) ) ;
#16791 = DIRECTION ( 'NONE',  ( -0.000000000000000000, -1.000000000000000000, -0.000000000000000000 ) ) ;
#16792 = VECTOR ( 'NONE', #940, 1000.000000000000000 ) ;
#16793 = CARTESIAN_POINT ( 'NONE',  ( 10.00000000000000000, 363.9544815475646260, -322.6258333628447872 ) ) ;
#16794 = FACE_OUTER_BOUND ( 'NONE', #5252, .T. ) ;
#16795 = ORIENTED_EDGE ( 'NONE', *, *, #289, .T. ) ;
#16796 = CARTESIAN_POINT ( 'NONE',  ( 2.265596578422603396E-15, 8.000000000000000000, 18.50000000000000000 ) ) ;
#16797 = AXIS2_PLACEMENT_3D ( 'NONE', #12060, #3041, #14548 ) ;
#16798 =( GEOMETRIC_REPRESENTATION_CONTEXT ( 3 ) GLOBAL_UNCERTAINTY_ASSIGNED_CONTEXT ( ( #2281 ) ) GLOBAL_UNIT_ASSIGNED_CONTEXT ( ( #3261, #16393, #3595 ) ) REPRESENTATION_CONTEXT ( 'NONE', 'WORKASPACE' ) );
#16799 = DIRECTION ( 'NONE',  ( 1.000000000000000000, -0.000000000000000000, -0.000000000000000000 ) ) ;
#16800 = PLANE ( 'NONE',  #8593 ) ;
#16801 = VECTOR ( 'NONE', #1576, 1000.000000000000000 ) ;
#16802 = ORIENTED_EDGE ( 'NONE', *, *, #5095, .T. ) ;
#16803 = CARTESIAN_POINT ( 'NONE',  ( -33.00000000000000000, 10.00000000000000000, -22.00000000000000355 ) ) ;
#16804 = VECTOR ( 'NONE', #6035, 1000.000000000000000 ) ;
#16805 = DIRECTION ( 'NONE',  ( 0.000000000000000000, 0.000000000000000000, 1.000000000000000000 ) ) ;
#16806 = ORIENTED_EDGE ( 'NONE', *, *, #7608, .F. ) ;
#16807 = PLANE ( 'NONE',  #3301 ) ;
#16808 = VECTOR ( 'NONE', #10349, 1000.000000000000000 ) ;
#16809 = FACE_OUTER_BOUND ( 'NONE', #3519, .T. ) ;
#16810 = DIRECTION ( 'NONE',  ( -0.000000000000000000, -0.000000000000000000, 1.000000000000000000 ) ) ;
#16811 = DIRECTION ( 'NONE',  ( 0.000000000000000000, 1.000000000000000000, 0.000000000000000000 ) ) ;
#16812 = ADVANCED_FACE ( 'NONE', ( #12577 ), #2177, .F. ) ;
#16813 = DIRECTION ( 'NONE',  ( -0.000000000000000000, -1.000000000000000000, -0.000000000000000000 ) ) ;
#16814 = CARTESIAN_POINT ( 'NONE',  ( 36.99999999999999289, 10.00000000000000000, 22.99999999999999645 ) ) ;
#16815 = LINE ( 'NONE', #5054, #4444 ) ;
#16816 = ORIENTED_EDGE ( 'NONE', *, *, #14479, .T. ) ;
#16817 = AXIS2_PLACEMENT_3D ( 'NONE', #15717, #2406, #6426 ) ;
#16818 = DIRECTION ( 'NONE',  ( 0.000000000000000000, 0.000000000000000000, -1.000000000000000000 ) ) ;
#16819 = CONTEXT_DEPENDENT_SHAPE_REPRESENTATION ( #6644, #9764 ) ;
#16820 = AXIS2_PLACEMENT_3D ( 'NONE', #2410, #11691, #12816 ) ;
#16821 = ADVANCED_FACE ( 'NONE', ( #4840 ), #7327, .F. ) ;
#16822 =( GEOMETRIC_REPRESENTATION_CONTEXT ( 3 ) GLOBAL_UNCERTAINTY_ASSIGNED_CONTEXT ( ( #10188 ) ) GLOBAL_UNIT_ASSIGNED_CONTEXT ( ( #15301, #12721, #8604 ) ) REPRESENTATION_CONTEXT ( 'NONE', 'WORKASPACE' ) );
#16823 = ORIENTED_EDGE ( 'NONE', *, *, #10574, .T. ) ;
#16824 = AXIS2_PLACEMENT_3D ( 'NONE', #11479, #16711, #4944 ) ;
#16825 = PLANE ( 'NONE',  #2803 ) ;
#16826 = CARTESIAN_POINT ( 'NONE',  ( -34.99999999999998579, -20.00000000000000000, 18.50000000000000355 ) ) ;
#16827 = CIRCLE ( 'NONE', #11903, 4.999999999999997335 ) ;
#16828 = FACE_OUTER_BOUND ( 'NONE', #4549, .T. ) ;
#16829 = VERTEX_POINT ( 'NONE', #12326 ) ;
#16830 = DIRECTION ( 'NONE',  ( 0.000000000000000000, 1.000000000000000000, 0.000000000000000000 ) ) ;
#16831 = DIRECTION ( 'NONE',  ( -0.000000000000000000, -1.000000000000000000, -0.000000000000000000 ) ) ;
#16832 = ORIENTED_EDGE ( 'NONE', *, *, #11006, .F. ) ;
#16833 =( GEOMETRIC_REPRESENTATION_CONTEXT ( 3 ) GLOBAL_UNCERTAINTY_ASSIGNED_CONTEXT ( ( #2112 ) ) GLOBAL_UNIT_ASSIGNED_CONTEXT ( ( #15978, #450, #9371 ) ) REPRESENTATION_CONTEXT ( 'NONE', 'WORKASPACE' ) );
#16834 = AXIS2_PLACEMENT_3D ( 'NONE', #14874, #3111, #16159 ) ;
#16835 = EDGE_CURVE ( 'NONE', #12822, #8007, #15065, .T. ) ;
#16836 = CARTESIAN_POINT ( 'NONE',  ( 2.625000000000000000, 0.000000000000000000, 0.000000000000000000 ) ) ;
#16837 = CONICAL_SURFACE ( 'NONE', #8362, 0.9999999999999950040, 1.029744258676644320 ) ;
#16838 = ORIENTED_EDGE ( 'NONE', *, *, #14805, .F. ) ;
#16839 = ORIENTED_EDGE ( 'NONE', *, *, #6662, .T. ) ;
#16840 = CARTESIAN_POINT ( 'NONE',  ( -20.99999999999999645, 19.00000000000000000, -31.00000000000003908 ) ) ;
#16841 = VECTOR ( 'NONE', #9728, 1000.000000000000000 ) ;
#16842 = ORIENTED_EDGE ( 'NONE', *, *, #1177, .F. ) ;
#16843 = EDGE_CURVE ( 'NONE', #13853, #6401, #818, .T. ) ;
#16844 = EDGE_CURVE ( 'NONE', #10385, #394, #3392, .T. ) ;
#16845 = EDGE_CURVE ( 'NONE', #16912, #7189, #3476, .T. ) ;
#16846 = EDGE_CURVE ( 'NONE', #15314, #14722, #379, .T. ) ;
#16847 = PRODUCT ( 'Servo-Axe', 'Servo-Axe', '', ( #3277 ) ) ;
#16848 = ORIENTED_EDGE ( 'NONE', *, *, #14231, .F. ) ;
#16849 = ORIENTED_EDGE ( 'NONE', *, *, #2425, .T. ) ;
#16850 = DIRECTION ( 'NONE',  ( -0.000000000000000000, -1.000000000000000000, -0.000000000000000000 ) ) ;
#16851 = AXIS2_PLACEMENT_3D ( 'NONE', #15801, #15879, #1632 ) ;
#16852 = DIRECTION ( 'NONE',  ( -1.000000000000000000, 0.000000000000000000, 0.000000000000000000 ) ) ;
#16853 = LINE ( 'NONE', #15322, #16552 ) ;
#16854 = ORIENTED_EDGE ( 'NONE', *, *, #3324, .T. ) ;
#16855 = AXIS2_PLACEMENT_3D ( 'NONE', #2458, #2543, #1176 ) ;
#16856 = DIRECTION ( 'NONE',  ( -3.854941057726249437E-16, -0.000000000000000000, 1.000000000000000000 ) ) ;
#16857 = CARTESIAN_POINT ( 'NONE',  ( 0.000000000000000000, 374.2147300931088694, -220.2054496871573974 ) ) ;
#16858 = LINE ( 'NONE', #16685, #12701 ) ;
#16859 = ORIENTED_EDGE ( 'NONE', *, *, #11959, .F. ) ;
#16860 = CARTESIAN_POINT ( 'NONE',  ( 3.000000000000000000, 41.00000000000000711, 9.013878188659973034 ) ) ;
#16861 = DIRECTION ( 'NONE',  ( -0.000000000000000000, -1.000000000000000000, -0.000000000000000000 ) ) ;
#16862 = ORIENTED_EDGE ( 'NONE', *, *, #13536, .T. ) ;
#16863 = LINE ( 'NONE', #15656, #11798 ) ;
#16864 = ORIENTED_EDGE ( 'NONE', *, *, #7342, .T. ) ;
#16865 = EDGE_CURVE ( 'NONE', #6188, #352, #11338, .T. ) ;
#16866 = LINE ( 'NONE', #3570, #4819 ) ;
#16867 = VECTOR ( 'NONE', #12672, 1000.000000000000000 ) ;
#16868 = EDGE_CURVE ( 'NONE', #15081, #4414, #8539, .T. ) ;
#16869 = ORIENTED_EDGE ( 'NONE', *, *, #9737, .T. ) ;
#16870 = VERTEX_POINT ( 'NONE', #2008 ) ;
#16871 = LINE ( 'NONE', #9060, #11579 ) ;
#16872 = DIRECTION ( 'NONE',  ( -1.000000000000000000, 0.000000000000000000, 0.000000000000000000 ) ) ;
#16873 = ORIENTED_EDGE ( 'NONE', *, *, #16745, .F. ) ;
#16874 = DIRECTION ( 'NONE',  ( -0.000000000000000000, -1.000000000000000000, -0.000000000000000000 ) ) ;
#16875 = LINE ( 'NONE', #1337, #11895 ) ;
#16876 = DIRECTION ( 'NONE',  ( 0.000000000000000000, 0.000000000000000000, -1.000000000000000000 ) ) ;
#16877 = TOROIDAL_SURFACE ( 'NONE', #3193, 4.695405383895982609, 9.000000000000000000 ) ;
#16878 = PLANE ( 'NONE',  #14729 ) ;
#16879 = DIRECTION ( 'NONE',  ( 8.673617379884027583E-16, 0.000000000000000000, -1.000000000000000000 ) ) ;
#16880 = CARTESIAN_POINT ( 'NONE',  ( 17.00000000000000711, 380.0000000000000000, -17.00000000000000355 ) ) ;
#16881 = CARTESIAN_POINT ( 'NONE',  ( -20.99999999999999645, 19.00000000000000000, -35.00000000000000711 ) ) ;
#16883 = ORIENTED_EDGE ( 'NONE', *, *, #2341, .F. ) ;
#16882 = VERTEX_POINT ( 'NONE', #7240 ) ;
#16884 = CARTESIAN_POINT ( 'NONE',  ( -270.0000000000000000, 512.1906115401388888, -11.00000000000000000 ) ) ;
#16885 = VECTOR ( 'NONE', #4126, 1000.000000000000000 ) ;
#16886 = DIRECTION ( 'NONE',  ( 6.123031769111888756E-17, -1.000000000000000000, -3.749151804555344967E-33 ) ) ;
#16887 = VECTOR ( 'NONE', #7693, 999.9999999999998863 ) ;
#16888 = DIRECTION ( 'NONE',  ( 0.000000000000000000, 0.000000000000000000, 1.000000000000000000 ) ) ;
#16889 = ORIENTED_EDGE ( 'NONE', *, *, #10223, .T. ) ;
#16890 = DIRECTION ( 'NONE',  ( -0.000000000000000000, -1.000000000000000000, 0.000000000000000000 ) ) ;
#16891 = DIRECTION ( 'NONE',  ( 0.000000000000000000, 0.6468954956981579629, -0.7625786632508376739 ) ) ;
#16892 = ORIENTED_EDGE ( 'NONE', *, *, #1958, .T. ) ;
#16893 = CARTESIAN_POINT ( 'NONE',  ( 55.99999999999989342, 523.2161522479893847, -590.5524132976893270 ) ) ;
#16894 = DIRECTION ( 'NONE',  ( -1.000000000000000000, 0.000000000000000000, 0.000000000000000000 ) ) ;
#16895 = CARTESIAN_POINT ( 'NONE',  ( 1.399999999999999911, 13.62500000000000000, 0.000000000000000000 ) ) ;
#16896 = LINE ( 'NONE', #15541, #14040 ) ;
#16897 = CIRCLE ( 'NONE', #13628, 6.473199999999998511 ) ;
#16898 = CIRCLE ( 'NONE', #15819, 13.69540538389601991 ) ;
#16899 = FILL_AREA_STYLE_COLOUR ( '', #7134 ) ;
#16900 = DIRECTION ( 'NONE',  ( 0.000000000000000000, 0.000000000000000000, -1.000000000000000000 ) ) ;
#16901 = CARTESIAN_POINT ( 'NONE',  ( -26.00000000000000000, 19.00000000000000000, 40.00000000000001421 ) ) ;
#16902 = EDGE_LOOP ( 'NONE', ( #360, #16415, #5766, #11265 ) ) ;
#16903 = CYLINDRICAL_SURFACE ( 'NONE', #6690, 13.69540538389601991 ) ;
#16904 = PLANE ( 'NONE',  #8844 ) ;
#16905 = CIRCLE ( 'NONE', #9256, 5.000000000000004441 ) ;
#16906 = ORIENTED_EDGE ( 'NONE', *, *, #9912, .T. ) ;
#16907 = EDGE_CURVE ( 'NONE', #15487, #15887, #8603, .T. ) ;
#16908 = VECTOR ( 'NONE', #15995, 1000.000000000000114 ) ;
#16909 = DIRECTION ( 'NONE',  ( 7.213771534993946619E-17, 0.09950371902098976984, 0.9950371902099900412 ) ) ;
#16910 = DIRECTION ( 'NONE',  ( 0.000000000000000000, 0.000000000000000000, -1.000000000000000000 ) ) ;
#16911 = DIRECTION ( 'NONE',  ( -1.156482317317881191E-15, 0.000000000000000000, -1.000000000000000000 ) ) ;
#16912 = VERTEX_POINT ( 'NONE', #8637 ) ;
#16913 = CARTESIAN_POINT ( 'NONE',  ( 5.162501635565829972, 0.000000000000000000, 0.000000000000000000 ) ) ;
#16914 = DIRECTION ( 'NONE',  ( -0.000000000000000000, 1.000000000000000000, -0.000000000000000000 ) ) ;
#16915 = VERTEX_POINT ( 'NONE', #2257 ) ;
#16916 = EDGE_CURVE ( 'NONE', #4130, #3064, #14360, .T. ) ;
#16917 = CARTESIAN_POINT ( 'NONE',  ( 10.00000000000000000, 435.2933666400819561, -525.1288175801793159 ) ) ;
#16918 = ORIENTED_EDGE ( 'NONE', *, *, #6816, .T. ) ;
#16919 = EDGE_LOOP ( 'NONE', ( #12714, #7054, #12556, #1671, #15986, #1478 ) ) ;
#16920 = AXIS2_PLACEMENT_3D ( 'NONE', #14422, #173, #6325 ) ;
#16921 = CARTESIAN_POINT ( 'NONE',  ( -40.00000000000000000, 68.00000000000000000, -25.99999999999999645 ) ) ;
#16922 = ORIENTED_EDGE ( 'NONE', *, *, #8848, .T. ) ;
#16923 = DIRECTION ( 'NONE',  ( 0.000000000000000000, 0.000000000000000000, -1.000000000000000000 ) ) ;
#16924 = VERTEX_POINT ( 'NONE', #10169 ) ;
#16925 = ORIENTED_EDGE ( 'NONE', *, *, #4793, .T. ) ;
#16926 = EDGE_CURVE ( 'NONE', #1542, #5265, #15727, .T. ) ;
#16927 = EDGE_CURVE ( 'NONE', #2869, #12856, #12719, .T. ) ;
#16928 = DIRECTION ( 'NONE',  ( -3.409610985204789889E-15, -0.9950371902099900412, 0.09950371902098964494 ) ) ;
#16929 = CARTESIAN_POINT ( 'NONE',  ( -3.000000000000000000, -1.836909530733565148E-16, 22.00000000000000000 ) ) ;
#16930 = EDGE_LOOP ( 'NONE', ( #5721, #9775, #3105, #2641 ) ) ;
#16931 = CARTESIAN_POINT ( 'NONE',  ( -26.00000000000002132, 0.000000000000000000, 40.00000000000000711 ) ) ;
#16932 = DIRECTION ( 'NONE',  ( -1.000000000000000000, 0.000000000000000000, -0.000000000000000000 ) ) ;
#16933 = ADVANCED_FACE ( 'NONE', ( #14124 ), #10259, .F. ) ;
#16934 = EDGE_CURVE ( 'NONE', #15703, #5778, #2290, .T. ) ;
#16935 = EDGE_CURVE ( 'NONE', #15084, #3282, #8968, .T. ) ;
#16936 = DIRECTION ( 'NONE',  ( -0.000000000000000000, -1.000000000000000000, -0.000000000000000000 ) ) ;
#16937 = ORIENTED_EDGE ( 'NONE', *, *, #13061, .F. ) ;
#16938 = LINE ( 'NONE', #10348, #4324 ) ;
#16939 = FACE_OUTER_BOUND ( 'NONE', #3649, .T. ) ;
#16940 = EDGE_LOOP ( 'NONE', ( #2530, #12801, #9902, #15638 ) ) ;
#16941 = CARTESIAN_POINT ( 'NONE',  ( 394.0000000000001137, 451.4647406485092915, -149.8062676851188257 ) ) ;
#16942 = ORIENTED_EDGE ( 'NONE', *, *, #9569, .F. ) ;
#16943 = PLANE ( 'NONE',  #449 ) ;
#16944 = VECTOR ( 'NONE', #7404, 1000.000000000000000 ) ;
#16945 = EDGE_LOOP ( 'NONE', ( #15854, #5420 ) ) ;
#16946 = ORIENTED_EDGE ( 'NONE', *, *, #12568, .T. ) ;
#16947 = DIRECTION ( 'NONE',  ( 0.000000000000000000, 0.000000000000000000, -1.000000000000000000 ) ) ;
#16948 = EDGE_CURVE ( 'NONE', #5421, #8165, #12749, .T. ) ;
#16949 = LINE ( 'NONE', #4004, #597 ) ;
#16950 = CARTESIAN_POINT ( 'NONE',  ( -25.99999999999999645, 68.00000000000000000, -39.99999999999999289 ) ) ;
#16951 = EDGE_LOOP ( 'NONE', ( #16937, #11705, #154, #9881 ) ) ;
#16952 = CARTESIAN_POINT ( 'NONE',  ( -22.99999999999999645, 68.00000000000000000, -31.00000000000005684 ) ) ;
#16953 = LINE ( 'NONE', #10525, #8881 ) ;
#16954 = ADVANCED_FACE ( 'NONE', ( #2344 ), #2424, .T. ) ;
#16955 = EDGE_CURVE ( 'NONE', #8117, #15832, #11092, .T. ) ;
#16956 = EDGE_CURVE ( 'NONE', #2103, #9177, #6199, .T. ) ;
#16957 = PLANE ( 'NONE',  #5760 ) ;
#16958 = EDGE_CURVE ( 'NONE', #8929, #5238, #7573, .T. ) ;
#16959 = CIRCLE ( 'NONE', #1328, 25.00000000000002132 ) ;
#16960 = CARTESIAN_POINT ( 'NONE',  ( 0.000000000000000000, 381.0487089519826895, 2.719601036885452502E-12 ) ) ;
#16961 = PLANE ( 'NONE',  #11300 ) ;
#16962 = CARTESIAN_POINT ( 'NONE',  ( -2.216159785453297477E-13, 106.2500000000000142, 3.000000000000000000 ) ) ;
#16963 = VECTOR ( 'NONE', #251, 1000.000000000000000 ) ;
#16964 = NEXT_ASSEMBLY_USAGE_OCCURRENCE ( 'NAUO1', ' ', ' ', #10102, #5043, $ ) ;
#16965 = NEXT_ASSEMBLY_USAGE_OCCURRENCE ( 'NAUO2', ' ', ' ', #10102, #5043, $ ) ;
#16966 = NEXT_ASSEMBLY_USAGE_OCCURRENCE ( 'NAUO3', ' ', ' ', #10102, #10624, $ ) ;
#16967 = NEXT_ASSEMBLY_USAGE_OCCURRENCE ( 'NAUO4', ' ', ' ', #10102, #10624, $ ) ;
#16968 = NEXT_ASSEMBLY_USAGE_OCCURRENCE ( 'NAUO5', ' ', ' ', #10102, #12202, $ ) ;
#16969 = NEXT_ASSEMBLY_USAGE_OCCURRENCE ( 'NAUO6', ' ', ' ', #10102, #16487, $ ) ;
#16970 = NEXT_ASSEMBLY_USAGE_OCCURRENCE ( 'NAUO7', ' ', ' ', #10102, #13142, $ ) ;
#16971 = NEXT_ASSEMBLY_USAGE_OCCURRENCE ( 'NAUO8', ' ', ' ', #10102, #4837, $ ) ;
#16972 = NEXT_ASSEMBLY_USAGE_OCCURRENCE ( 'NAUO9', ' ', ' ', #10102, #4837, $ ) ;
#16973 = NEXT_ASSEMBLY_USAGE_OCCURRENCE ( 'NAUO10', ' ', ' ', #10102, #9689, $ ) ;
#16974 = NEXT_ASSEMBLY_USAGE_OCCURRENCE ( 'NAUO11', ' ', ' ', #10102, #2213, $ ) ;
#16975 = NEXT_ASSEMBLY_USAGE_OCCURRENCE ( 'NAUO12', ' ', ' ', #10102, #12720, $ ) ;
#16976 = NEXT_ASSEMBLY_USAGE_OCCURRENCE ( 'NAUO13', ' ', ' ', #10102, #2741, $ ) ;
#16977 = NEXT_ASSEMBLY_USAGE_OCCURRENCE ( 'NAUO14', ' ', ' ', #2741, #10407, $ ) ;
#16978 = NEXT_ASSEMBLY_USAGE_OCCURRENCE ( 'NAUO15', ' ', ' ', #2741, #10407, $ ) ;
#16979 = NEXT_ASSEMBLY_USAGE_OCCURRENCE ( 'NAUO16', ' ', ' ', #2741, #7350, $ ) ;
#16980 = NEXT_ASSEMBLY_USAGE_OCCURRENCE ( 'NAUO17', ' ', ' ', #12202, #13469, $ ) ;
#16981 = NEXT_ASSEMBLY_USAGE_OCCURRENCE ( 'NAUO18', ' ', ' ', #12202, #14937, $ ) ;
#16982 = NEXT_ASSEMBLY_USAGE_OCCURRENCE ( 'NAUO19', ' ', ' ', #12202, #14195, $ ) ;
#16983 = NEXT_ASSEMBLY_USAGE_OCCURRENCE ( 'NAUO20', ' ', ' ', #12202, #6603, $ ) ;
#16984 = NEXT_ASSEMBLY_USAGE_OCCURRENCE ( 'NAUO21', ' ', ' ', #12202, #8102, $ ) ;
#16985 = NEXT_ASSEMBLY_USAGE_OCCURRENCE ( 'NAUO22', ' ', ' ', #12202, #4018, $ ) ;
#16986 = NEXT_ASSEMBLY_USAGE_OCCURRENCE ( 'NAUO23', ' ', ' ', #12202, #1808, $ ) ;
ENDSEC;
END-ISO-10303-21;
